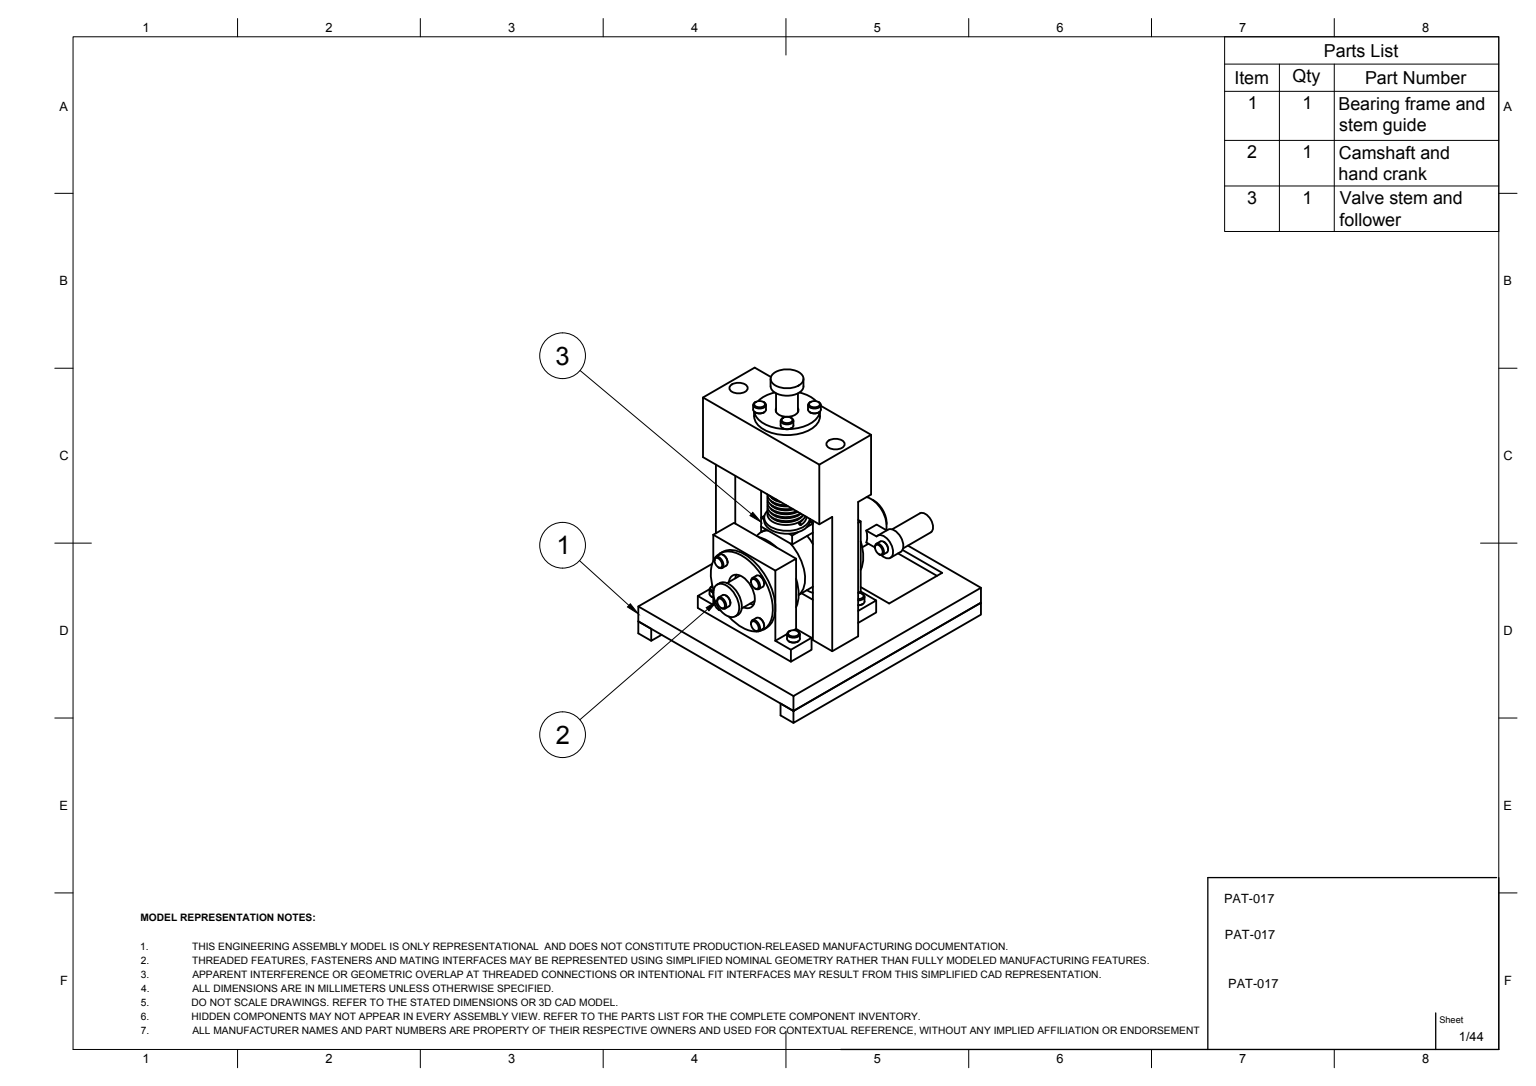
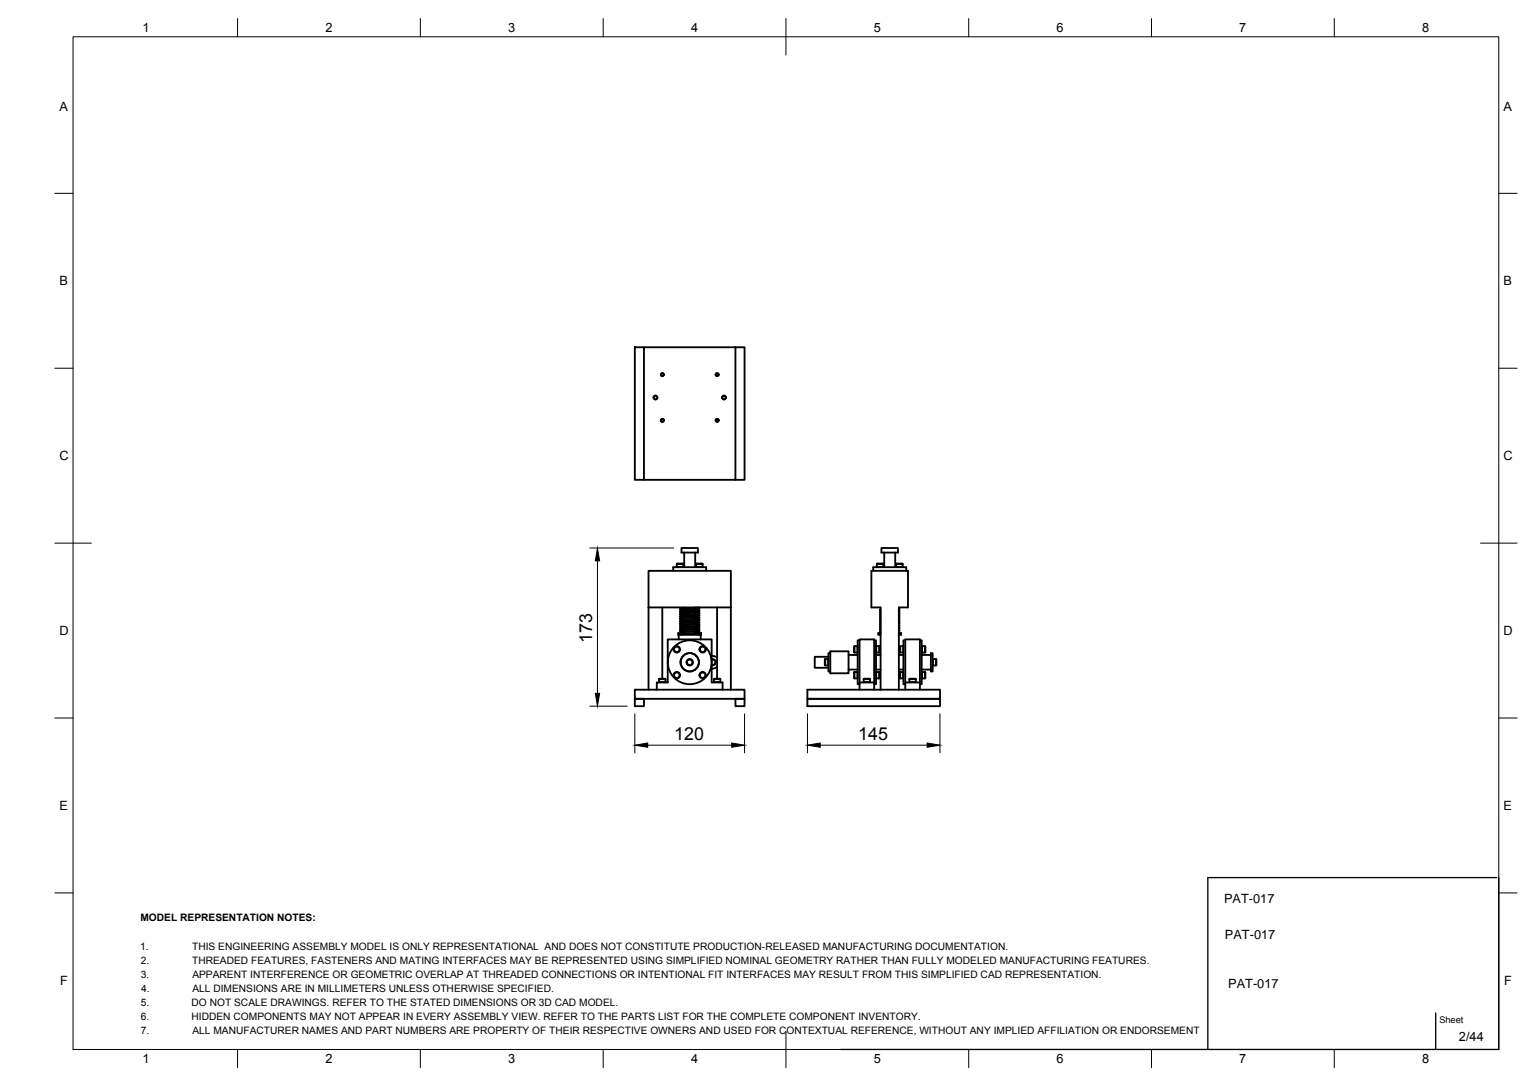
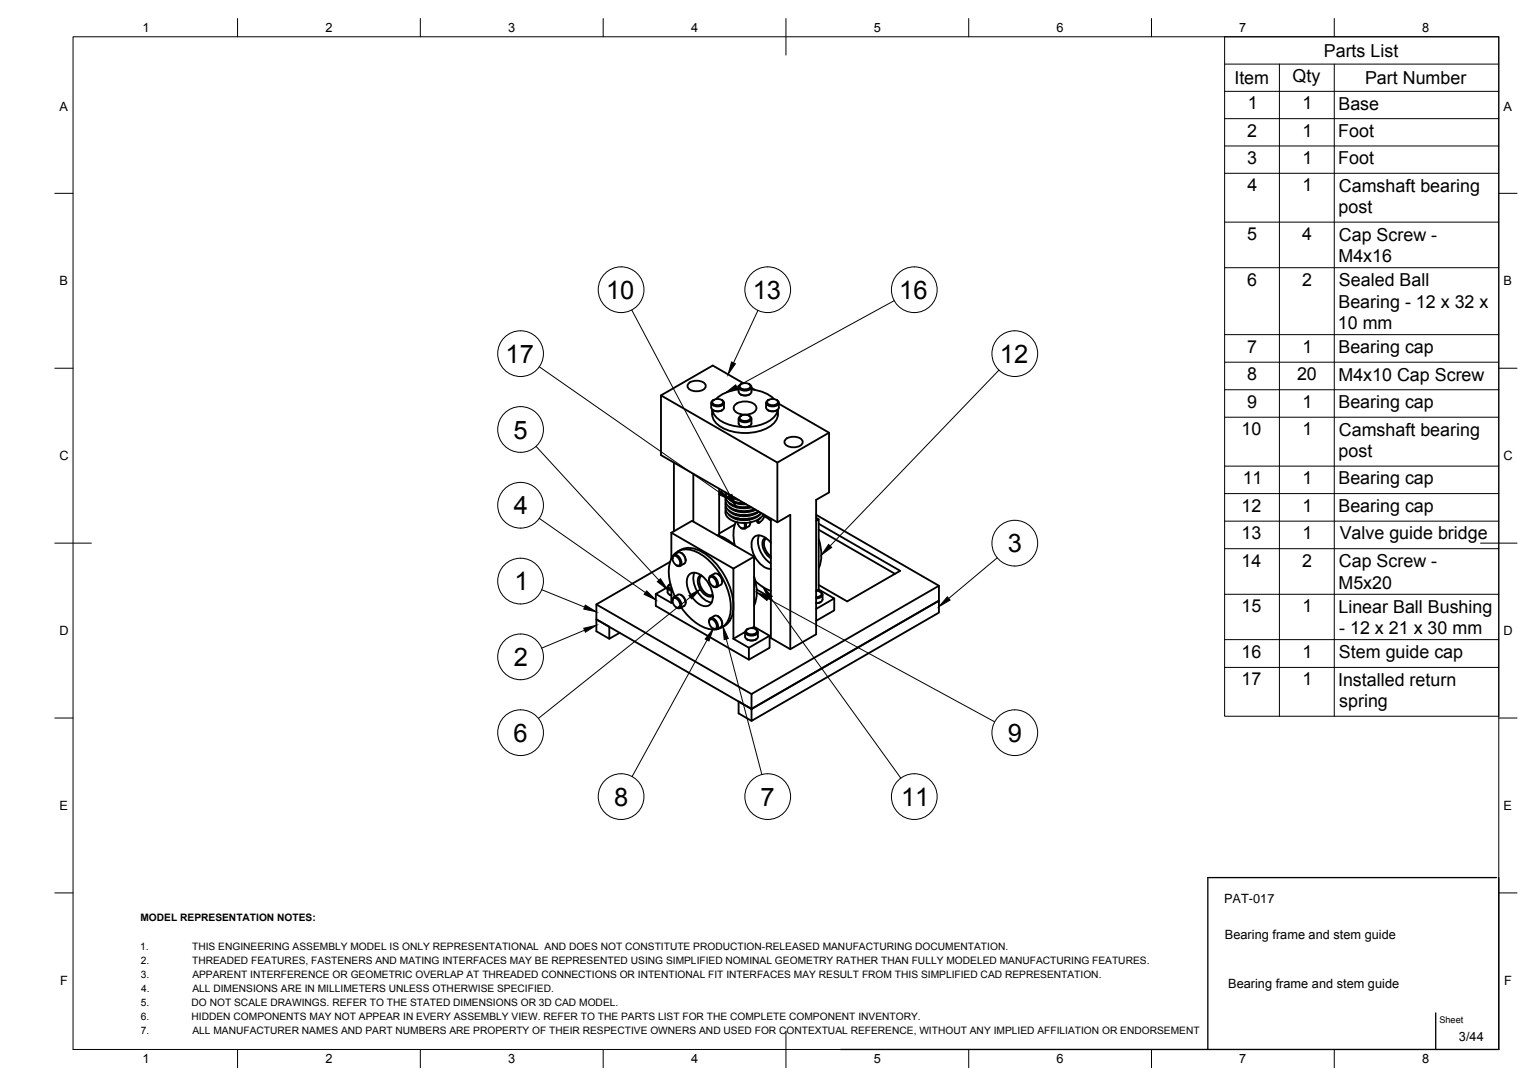
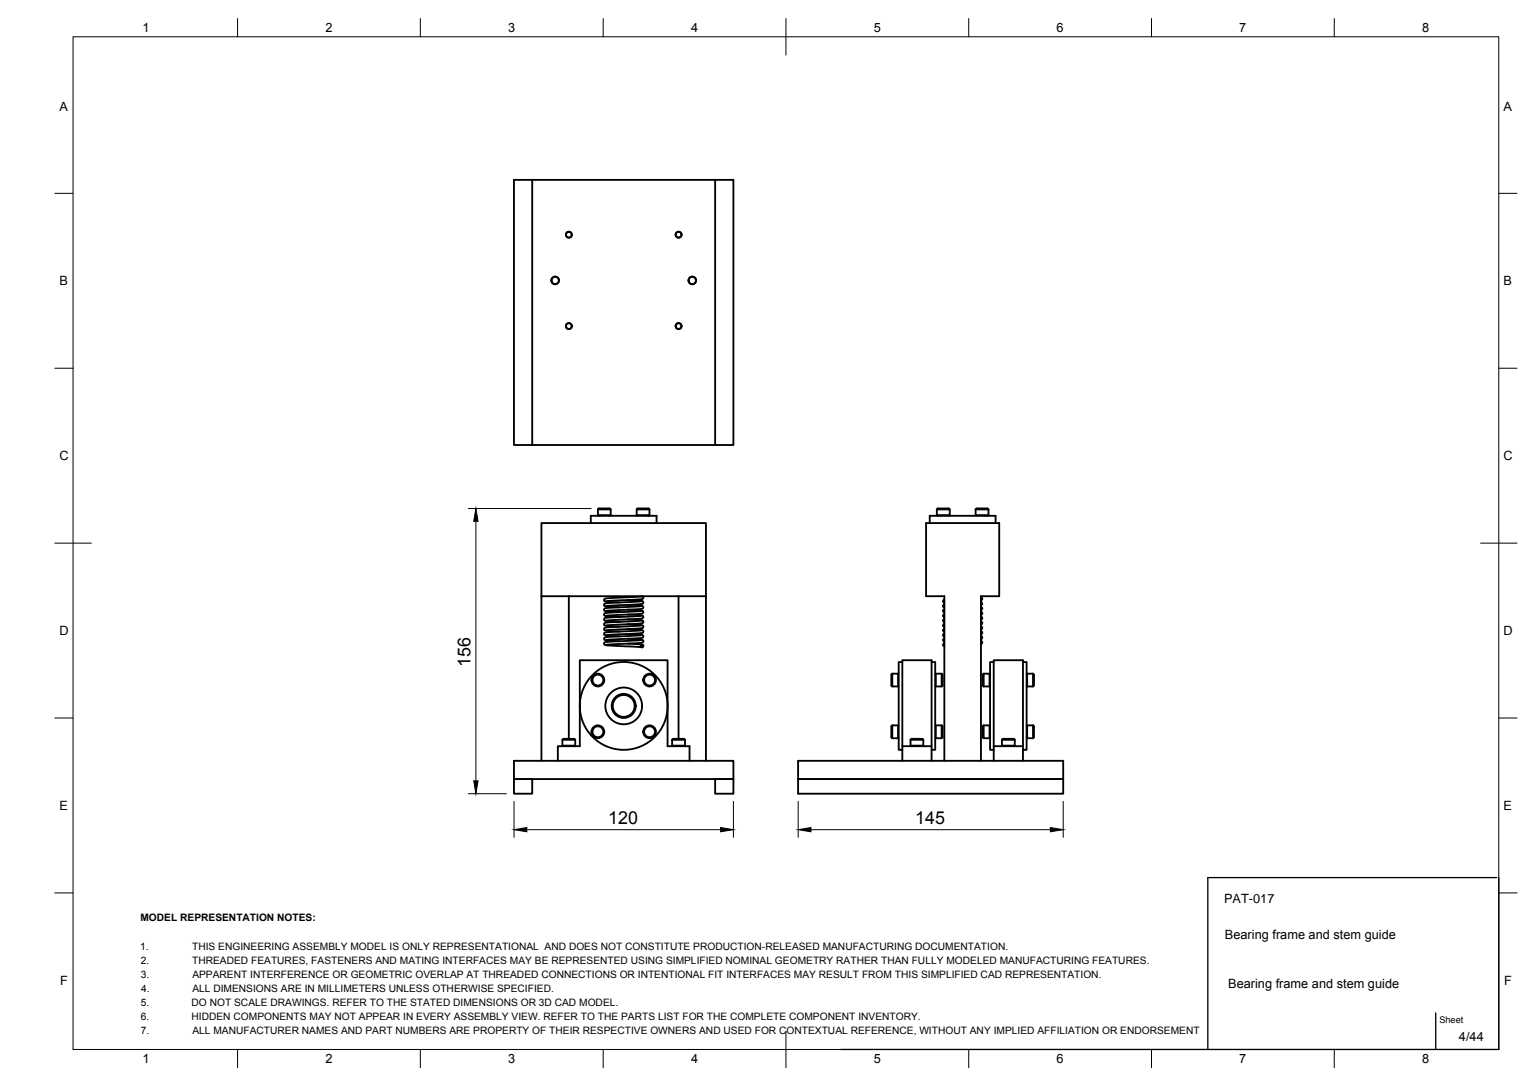
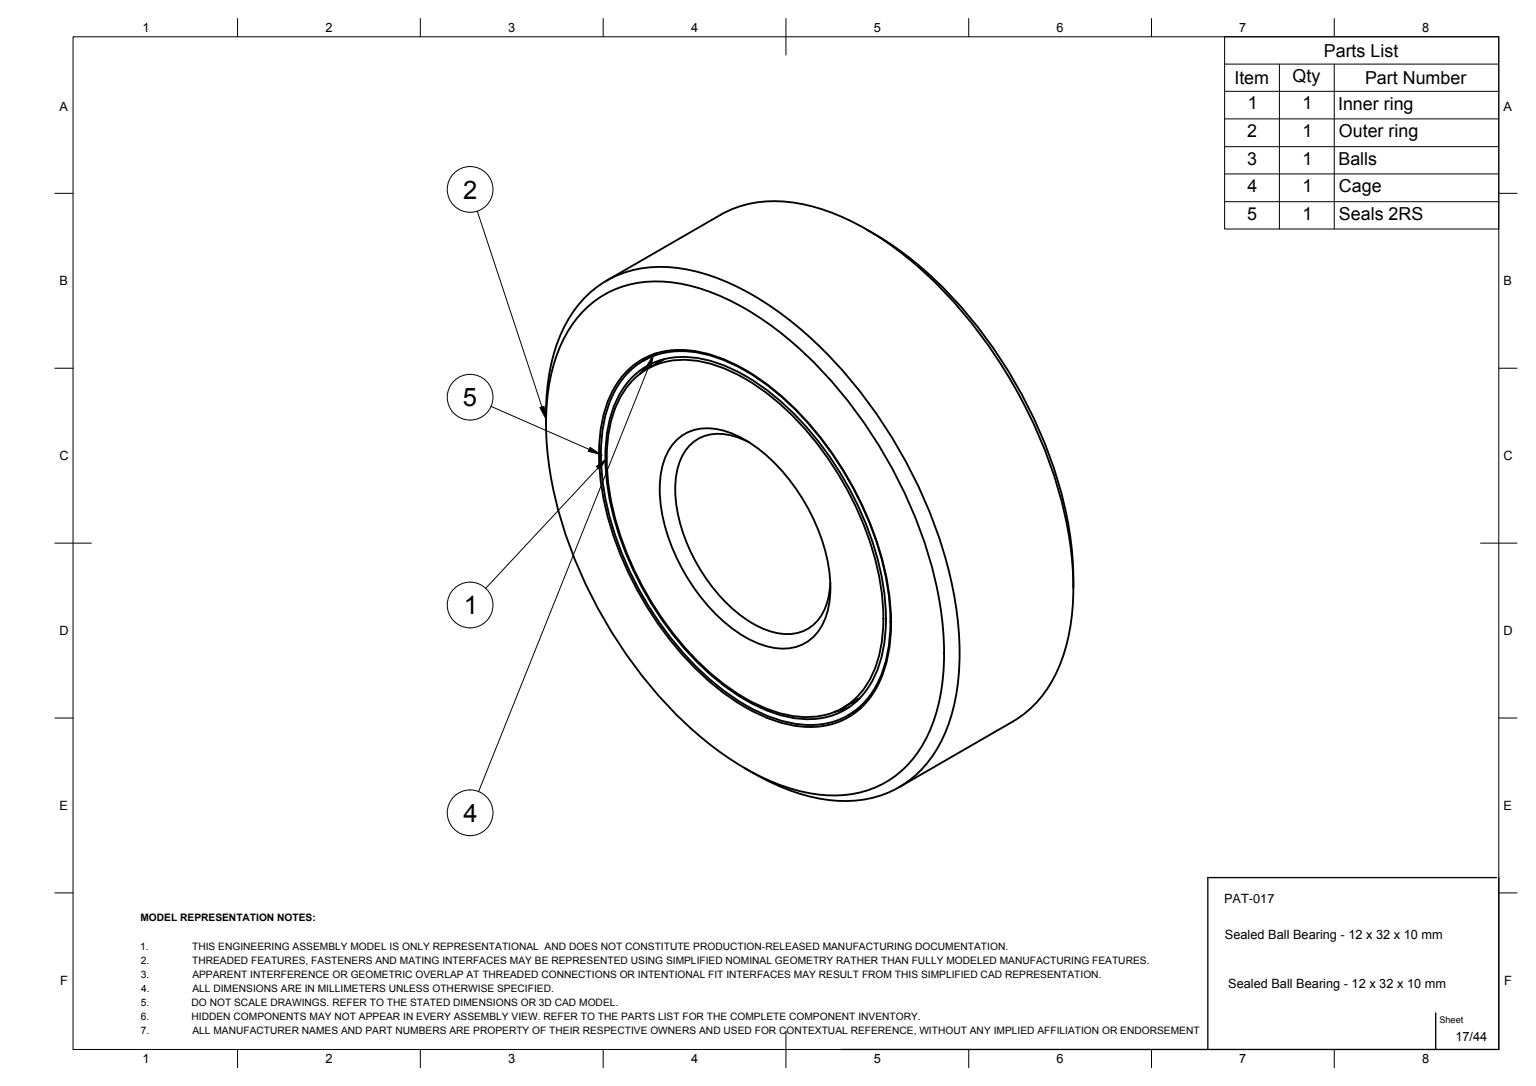
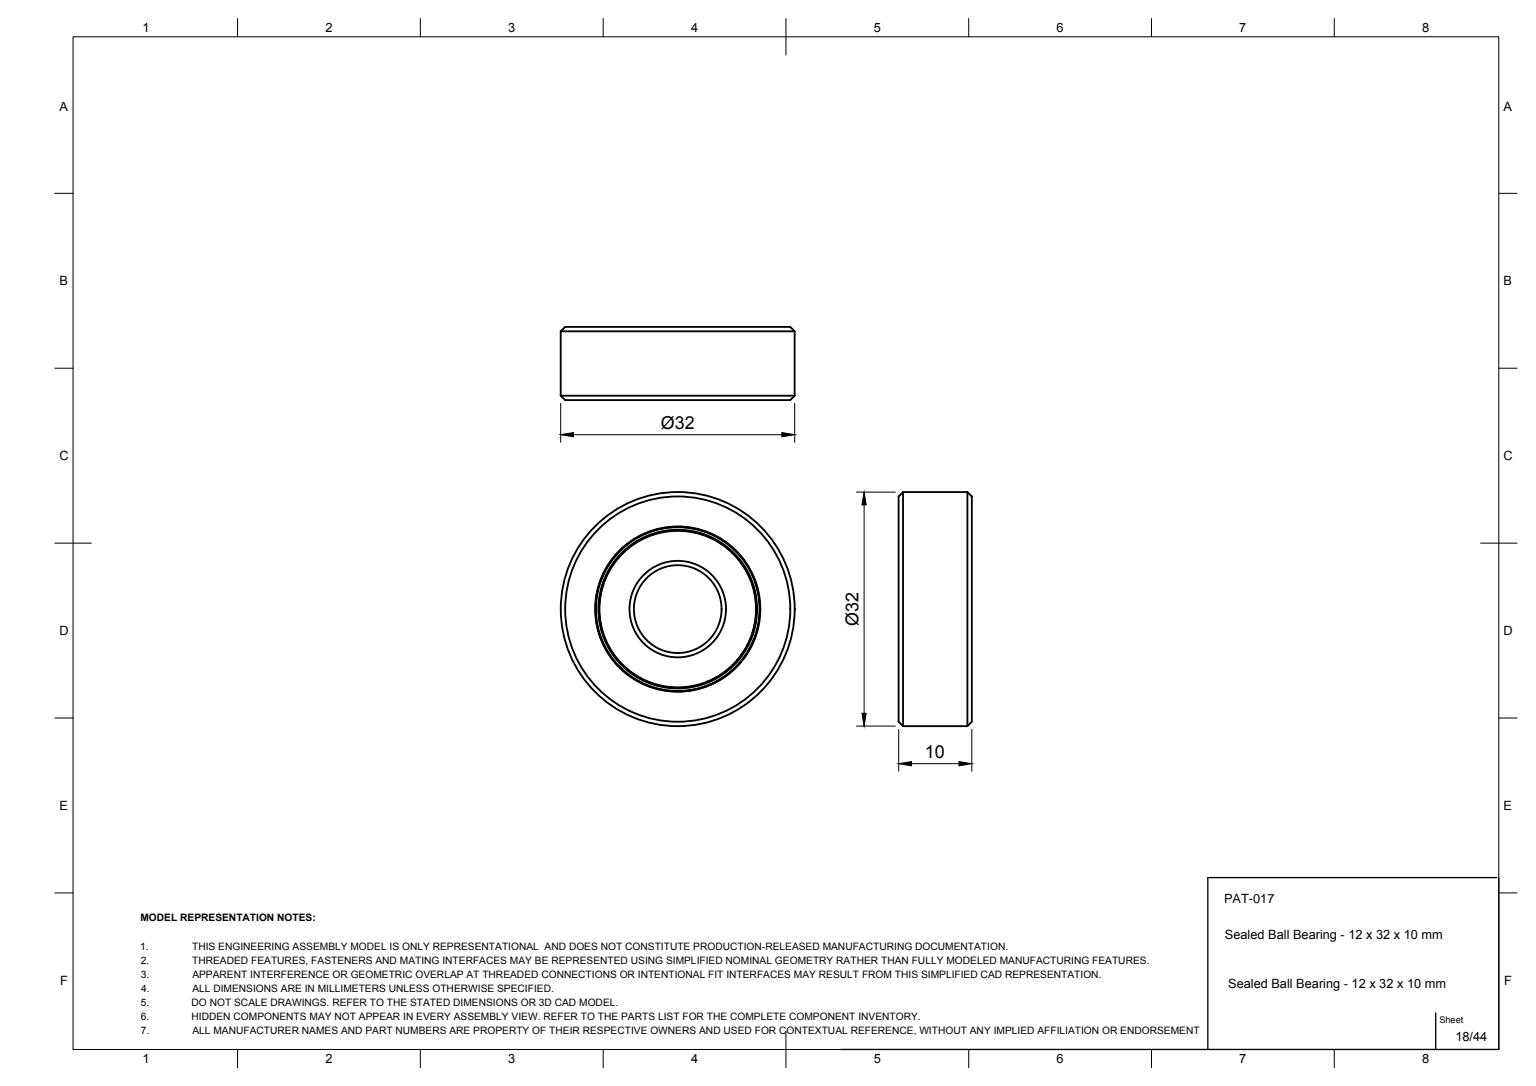
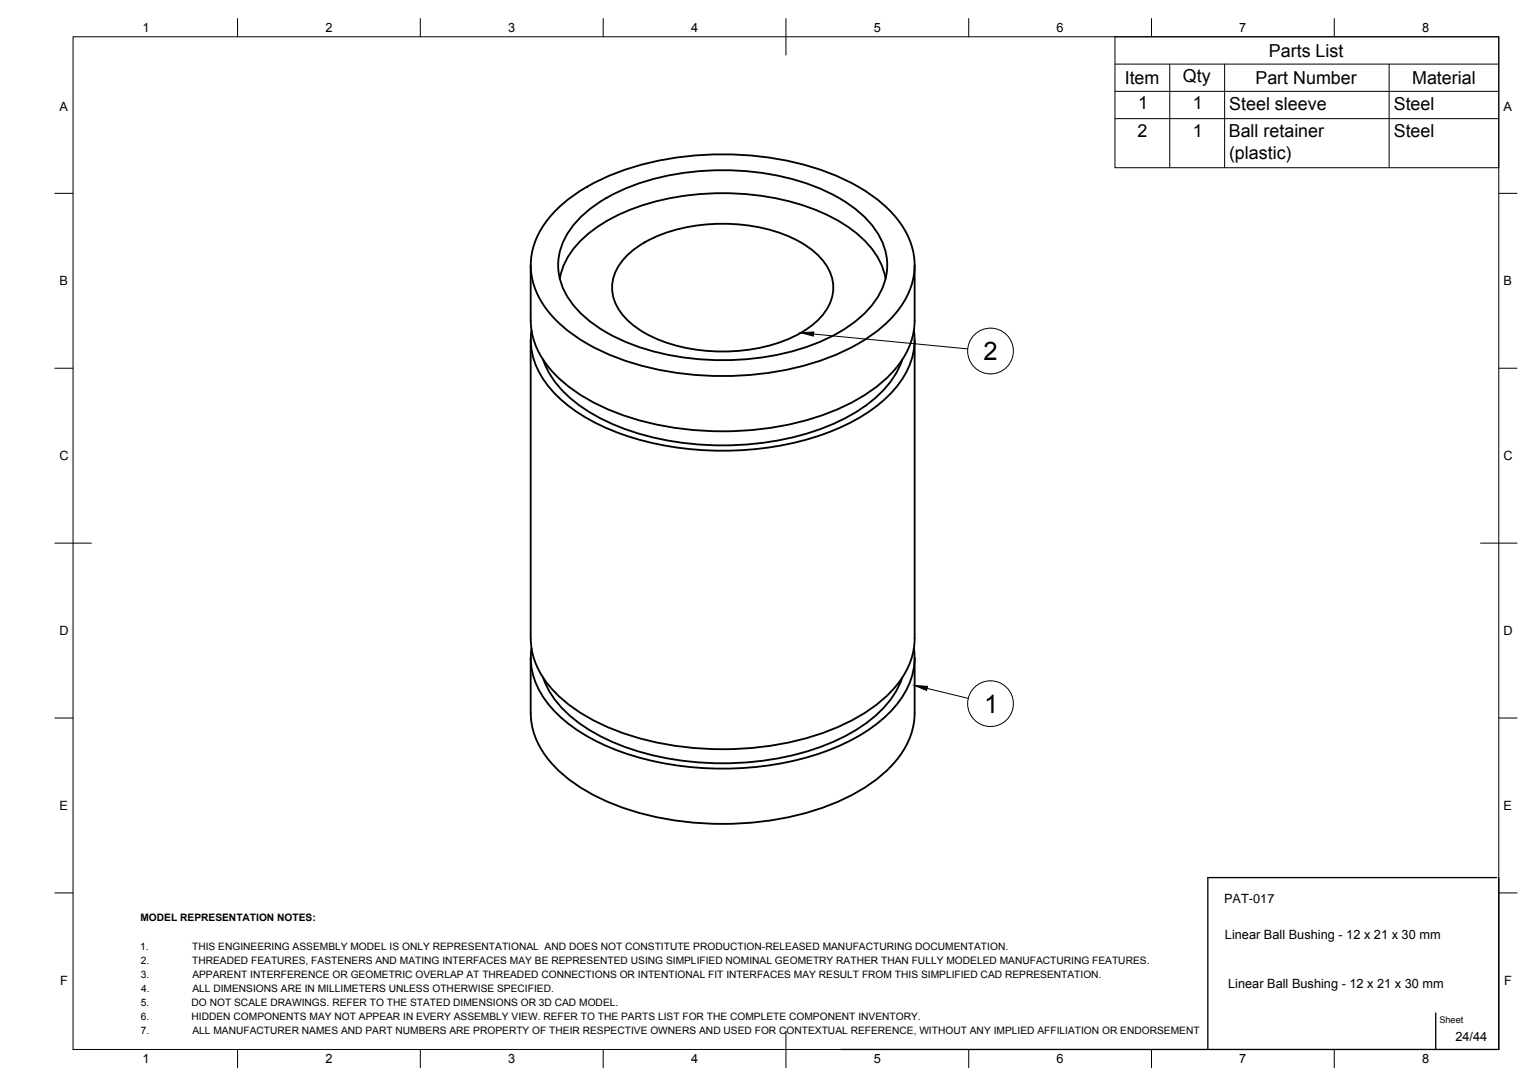
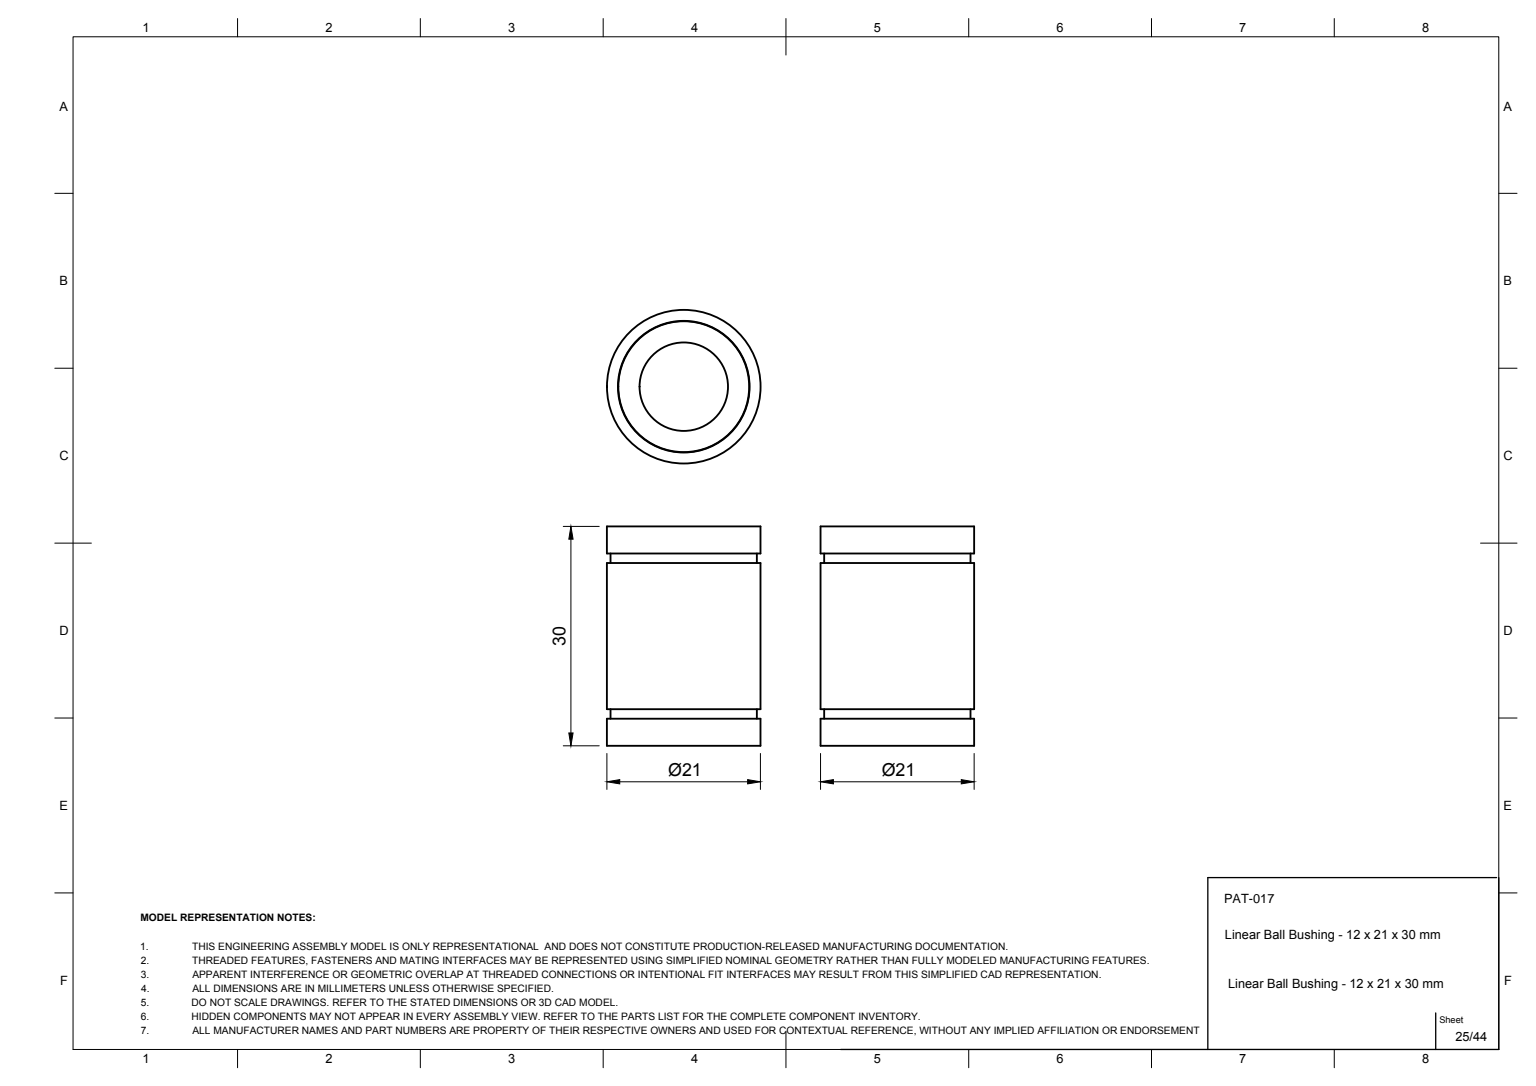
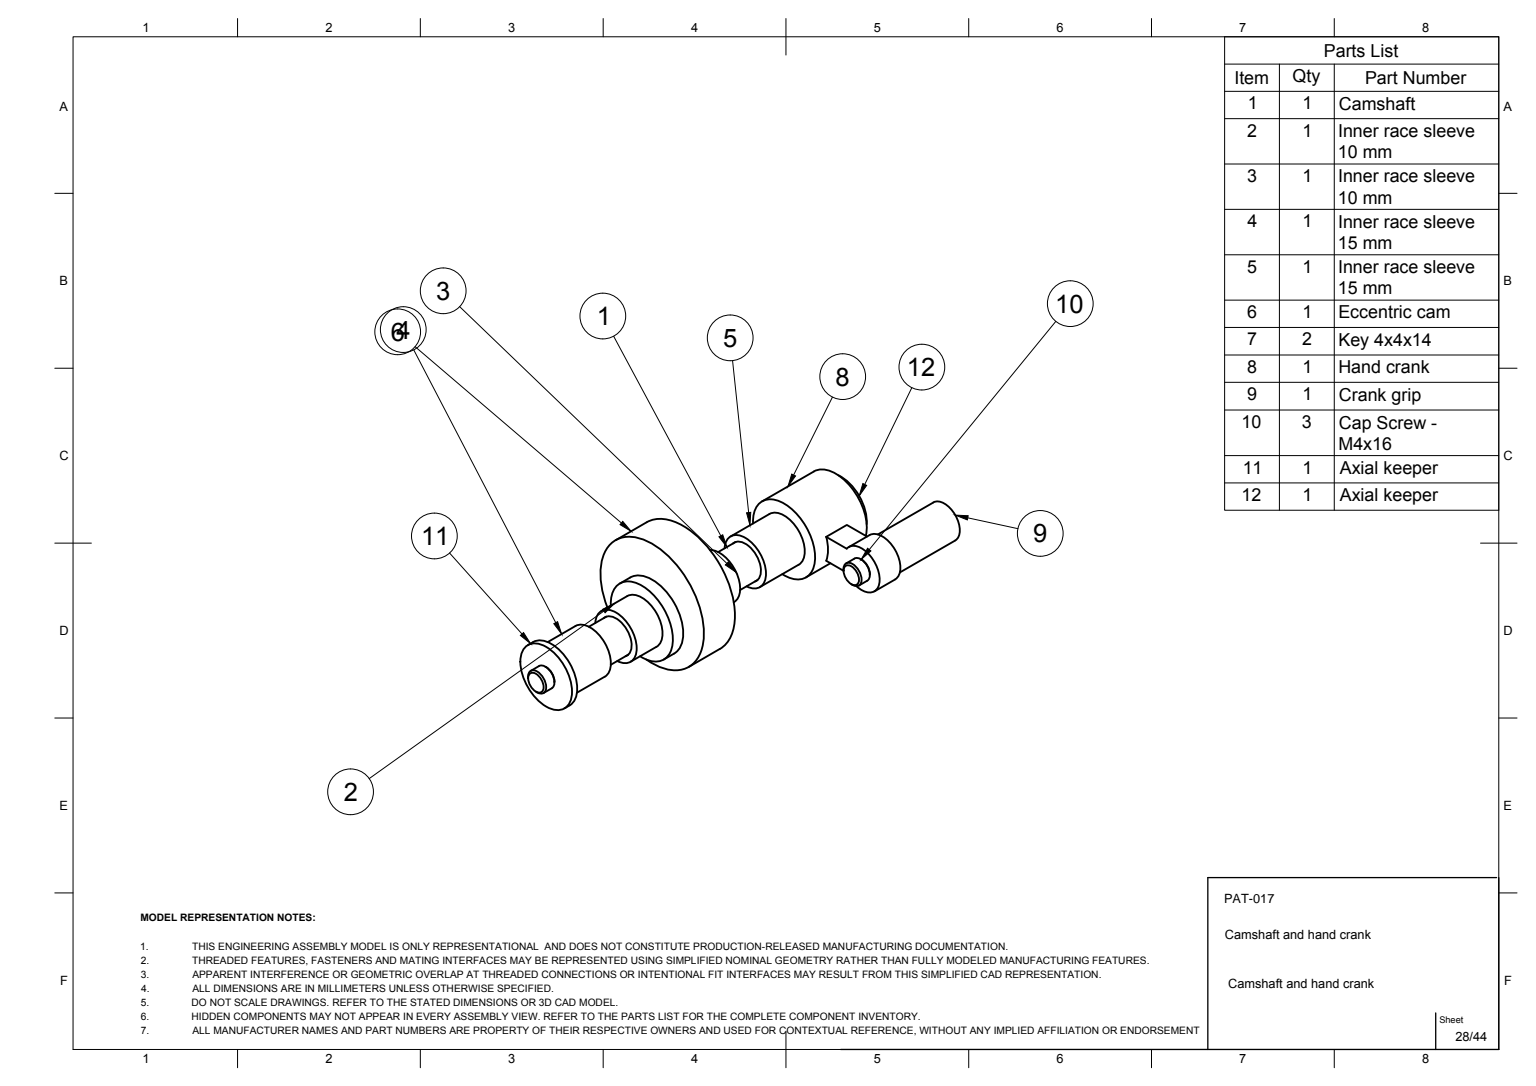
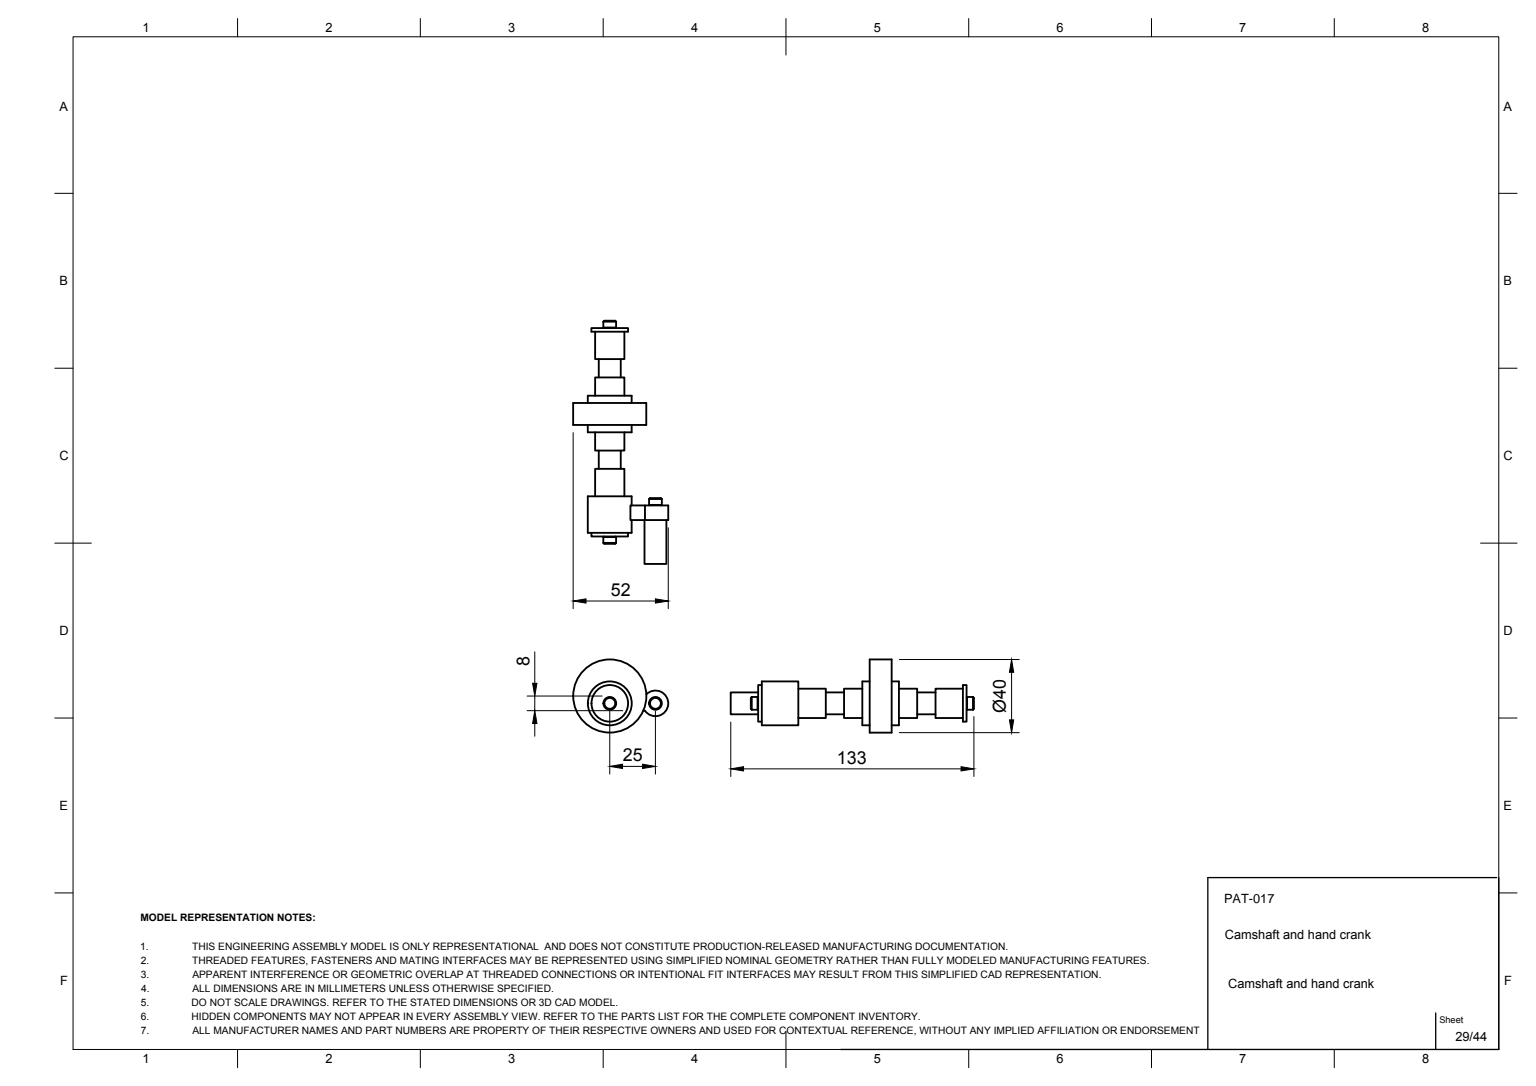
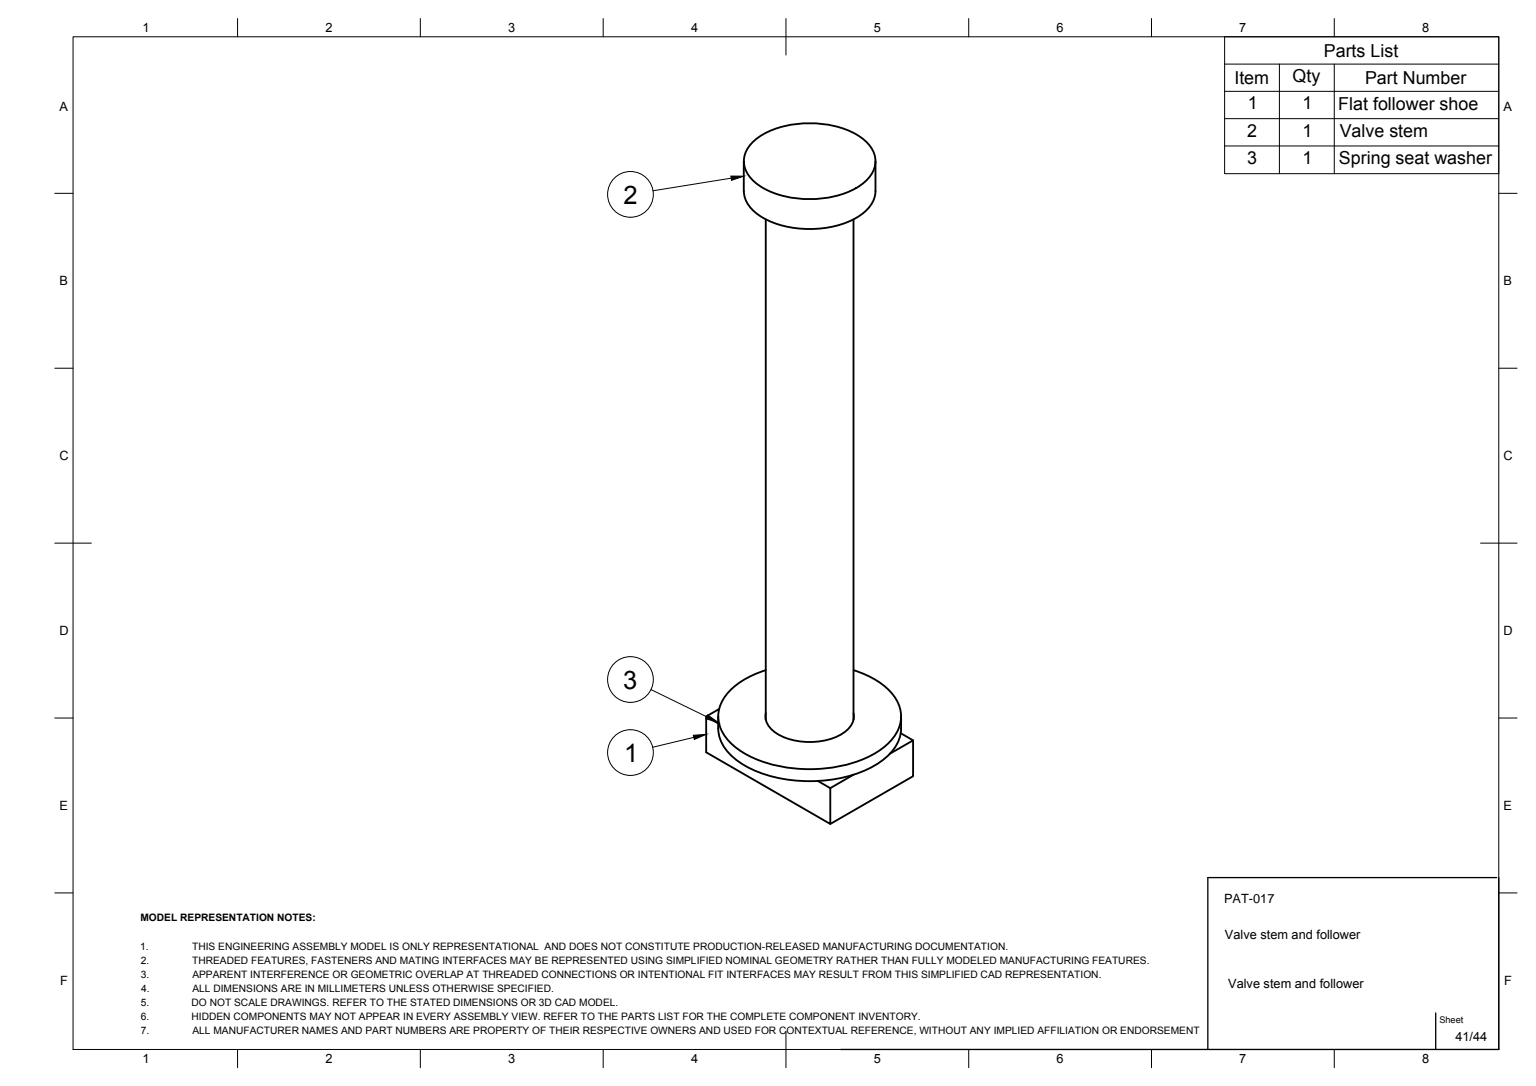
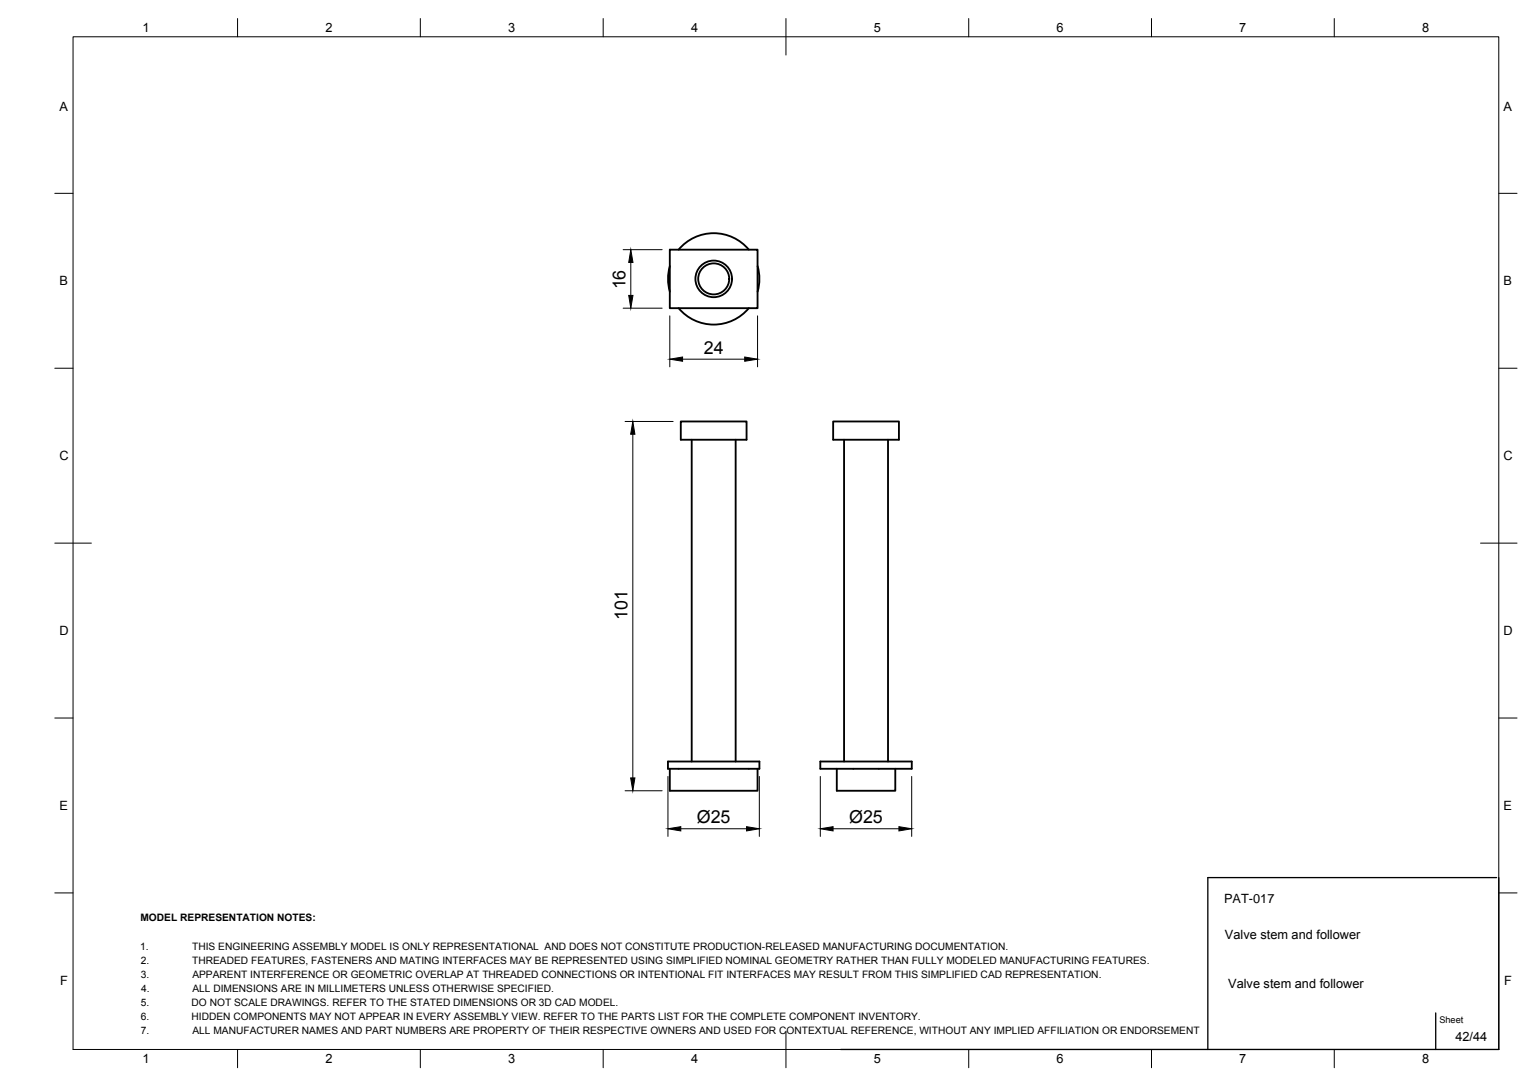
ISO-10303-21;
HEADER;
/* Generated by software containing ST-Developer
 * from STEP Tools, Inc. (www.steptools.com) 
 */

FILE_DESCRIPTION(
/* description */ ('Cam-and-follower valve demonstrator'),
/* implementation_level */ '2;1');

FILE_NAME(
/* name */ 'PAT-017',
/* time_stamp */ '2026-10-28T03:25:17-07:00',
/* author */ (''),
/* organization */ (''),
/* preprocessor_version */ 'ST-DEVELOPER v20.2',
/* originating_system */ 'Autodesk Translation Framework v15.17.0.0',
/* authorisation */ '');

FILE_SCHEMA (('AUTOMOTIVE_DESIGN { 1 0 10303 214 3 1 1 }'));
ENDSEC;

DATA;
#10=MECHANICAL_DESIGN_GEOMETRIC_PRESENTATION_REPRESENTATION('',(#412,#413,
#414,#415,#416,#417,#418,#419,#420,#421,#422,#423,#424,#425,#426,#427,#428,
#429,#430,#431,#432,#433,#434,#435,#436,#437,#438,#439,#440,#441,#442,#443,
#444,#445,#446,#447,#448,#449,#450,#451,#452,#453,#454),#12896);
#11=ORIENTED_CLOSED_SHELL('',*,#6204,.F.);
#12=ORIENTED_CLOSED_SHELL('',*,#6207,.F.);
#13=ORIENTED_CLOSED_SHELL('',*,#6221,.F.);
#14=BREP_WITH_VOIDS('Body1',#6203,(#11));
#15=BREP_WITH_VOIDS('Body1',#6208,(#12));
#16=BREP_WITH_VOIDS('Body1',#6220,(#13));
#17=ITEM_DEFINED_TRANSFORMATION($,$,#6915,#7037);
#18=ITEM_DEFINED_TRANSFORMATION($,$,#6935,#7038);
#19=ITEM_DEFINED_TRANSFORMATION($,$,#6955,#7039);
#20=ITEM_DEFINED_TRANSFORMATION($,$,#6970,#7040);
#21=ITEM_DEFINED_TRANSFORMATION($,$,#7020,#7041);
#22=ITEM_DEFINED_TRANSFORMATION($,$,#7069,#7118);
#23=ITEM_DEFINED_TRANSFORMATION($,$,#7101,#7119);
#24=ITEM_DEFINED_TRANSFORMATION($,$,#6624,#7318);
#25=ITEM_DEFINED_TRANSFORMATION($,$,#6654,#7319);
#26=ITEM_DEFINED_TRANSFORMATION($,$,#6661,#7320);
#27=ITEM_DEFINED_TRANSFORMATION($,$,#6668,#7321);
#28=ITEM_DEFINED_TRANSFORMATION($,$,#6700,#7322);
#29=ITEM_DEFINED_TRANSFORMATION($,$,#6725,#7323);
#30=ITEM_DEFINED_TRANSFORMATION($,$,#6750,#7324);
#31=ITEM_DEFINED_TRANSFORMATION($,$,#6782,#7325);
#32=ITEM_DEFINED_TRANSFORMATION($,$,#6807,#7326);
#33=ITEM_DEFINED_TRANSFORMATION($,$,#6832,#7327);
#34=ITEM_DEFINED_TRANSFORMATION($,$,#6884,#7328);
#35=ITEM_DEFINED_TRANSFORMATION($,$,#6909,#7329);
#36=ITEM_DEFINED_TRANSFORMATION($,$,#7292,#7330);
#37=ITEM_DEFINED_TRANSFORMATION($,$,#7292,#7331);
#38=ITEM_DEFINED_TRANSFORMATION($,$,#6914,#7332);
#39=ITEM_DEFINED_TRANSFORMATION($,$,#7120,#7333);
#40=ITEM_DEFINED_TRANSFORMATION($,$,#7120,#7334);
#41=ITEM_DEFINED_TRANSFORMATION($,$,#7120,#7335);
#42=ITEM_DEFINED_TRANSFORMATION($,$,#7120,#7336);
#43=ITEM_DEFINED_TRANSFORMATION($,$,#7120,#7337);
#44=ITEM_DEFINED_TRANSFORMATION($,$,#7120,#7338);
#45=ITEM_DEFINED_TRANSFORMATION($,$,#7120,#7339);
#46=ITEM_DEFINED_TRANSFORMATION($,$,#7120,#7340);
#47=ITEM_DEFINED_TRANSFORMATION($,$,#7292,#7341);
#48=ITEM_DEFINED_TRANSFORMATION($,$,#7292,#7342);
#49=ITEM_DEFINED_TRANSFORMATION($,$,#6914,#7343);
#50=ITEM_DEFINED_TRANSFORMATION($,$,#7120,#7344);
#51=ITEM_DEFINED_TRANSFORMATION($,$,#7120,#7345);
#52=ITEM_DEFINED_TRANSFORMATION($,$,#7120,#7346);
#53=ITEM_DEFINED_TRANSFORMATION($,$,#7120,#7347);
#54=ITEM_DEFINED_TRANSFORMATION($,$,#7120,#7348);
#55=ITEM_DEFINED_TRANSFORMATION($,$,#7120,#7349);
#56=ITEM_DEFINED_TRANSFORMATION($,$,#7120,#7350);
#57=ITEM_DEFINED_TRANSFORMATION($,$,#7120,#7351);
#58=ITEM_DEFINED_TRANSFORMATION($,$,#7042,#7352);
#59=ITEM_DEFINED_TRANSFORMATION($,$,#7042,#7353);
#60=ITEM_DEFINED_TRANSFORMATION($,$,#7068,#7354);
#61=ITEM_DEFINED_TRANSFORMATION($,$,#7120,#7355);
#62=ITEM_DEFINED_TRANSFORMATION($,$,#7120,#7356);
#63=ITEM_DEFINED_TRANSFORMATION($,$,#7120,#7357);
#64=ITEM_DEFINED_TRANSFORMATION($,$,#7120,#7358);
#65=ITEM_DEFINED_TRANSFORMATION($,$,#7145,#7359);
#66=ITEM_DEFINED_TRANSFORMATION($,$,#7173,#7360);
#67=ITEM_DEFINED_TRANSFORMATION($,$,#7182,#7361);
#68=ITEM_DEFINED_TRANSFORMATION($,$,#7191,#7362);
#69=ITEM_DEFINED_TRANSFORMATION($,$,#7200,#7363);
#70=ITEM_DEFINED_TRANSFORMATION($,$,#7209,#7364);
#71=ITEM_DEFINED_TRANSFORMATION($,$,#7229,#7365);
#72=ITEM_DEFINED_TRANSFORMATION($,$,#7253,#7366);
#73=ITEM_DEFINED_TRANSFORMATION($,$,#7263,#7367);
#74=ITEM_DEFINED_TRANSFORMATION($,$,#7272,#7368);
#75=ITEM_DEFINED_TRANSFORMATION($,$,#7281,#7369);
#76=ITEM_DEFINED_TRANSFORMATION($,$,#7281,#7370);
#77=ITEM_DEFINED_TRANSFORMATION($,$,#7292,#7371);
#78=ITEM_DEFINED_TRANSFORMATION($,$,#7292,#7372);
#79=ITEM_DEFINED_TRANSFORMATION($,$,#7292,#7373);
#80=ITEM_DEFINED_TRANSFORMATION($,$,#7375,#7408);
#81=ITEM_DEFINED_TRANSFORMATION($,$,#7385,#7409);
#82=ITEM_DEFINED_TRANSFORMATION($,$,#7399,#7410);
#83=ITEM_DEFINED_TRANSFORMATION($,$,#6623,#7411);
#84=ITEM_DEFINED_TRANSFORMATION($,$,#7144,#7412);
#85=ITEM_DEFINED_TRANSFORMATION($,$,#7374,#7413);
#86=(
REPRESENTATION_RELATIONSHIP($,$,#13069,#13068)
REPRESENTATION_RELATIONSHIP_WITH_TRANSFORMATION(#17)
SHAPE_REPRESENTATION_RELATIONSHIP()
);
#87=(
REPRESENTATION_RELATIONSHIP($,$,#13070,#13068)
REPRESENTATION_RELATIONSHIP_WITH_TRANSFORMATION(#18)
SHAPE_REPRESENTATION_RELATIONSHIP()
);
#88=(
REPRESENTATION_RELATIONSHIP($,$,#13071,#13068)
REPRESENTATION_RELATIONSHIP_WITH_TRANSFORMATION(#19)
SHAPE_REPRESENTATION_RELATIONSHIP()
);
#89=(
REPRESENTATION_RELATIONSHIP($,$,#13072,#13068)
REPRESENTATION_RELATIONSHIP_WITH_TRANSFORMATION(#20)
SHAPE_REPRESENTATION_RELATIONSHIP()
);
#90=(
REPRESENTATION_RELATIONSHIP($,$,#13073,#13068)
REPRESENTATION_RELATIONSHIP_WITH_TRANSFORMATION(#21)
SHAPE_REPRESENTATION_RELATIONSHIP()
);
#91=(
REPRESENTATION_RELATIONSHIP($,$,#13076,#13075)
REPRESENTATION_RELATIONSHIP_WITH_TRANSFORMATION(#22)
SHAPE_REPRESENTATION_RELATIONSHIP()
);
#92=(
REPRESENTATION_RELATIONSHIP($,$,#13077,#13075)
REPRESENTATION_RELATIONSHIP_WITH_TRANSFORMATION(#23)
SHAPE_REPRESENTATION_RELATIONSHIP()
);
#93=(
REPRESENTATION_RELATIONSHIP($,$,#13056,#13055)
REPRESENTATION_RELATIONSHIP_WITH_TRANSFORMATION(#24)
SHAPE_REPRESENTATION_RELATIONSHIP()
);
#94=(
REPRESENTATION_RELATIONSHIP($,$,#13057,#13055)
REPRESENTATION_RELATIONSHIP_WITH_TRANSFORMATION(#25)
SHAPE_REPRESENTATION_RELATIONSHIP()
);
#95=(
REPRESENTATION_RELATIONSHIP($,$,#13058,#13055)
REPRESENTATION_RELATIONSHIP_WITH_TRANSFORMATION(#26)
SHAPE_REPRESENTATION_RELATIONSHIP()
);
#96=(
REPRESENTATION_RELATIONSHIP($,$,#13059,#13055)
REPRESENTATION_RELATIONSHIP_WITH_TRANSFORMATION(#27)
SHAPE_REPRESENTATION_RELATIONSHIP()
);
#97=(
REPRESENTATION_RELATIONSHIP($,$,#13060,#13055)
REPRESENTATION_RELATIONSHIP_WITH_TRANSFORMATION(#28)
SHAPE_REPRESENTATION_RELATIONSHIP()
);
#98=(
REPRESENTATION_RELATIONSHIP($,$,#13061,#13055)
REPRESENTATION_RELATIONSHIP_WITH_TRANSFORMATION(#29)
SHAPE_REPRESENTATION_RELATIONSHIP()
);
#99=(
REPRESENTATION_RELATIONSHIP($,$,#13062,#13055)
REPRESENTATION_RELATIONSHIP_WITH_TRANSFORMATION(#30)
SHAPE_REPRESENTATION_RELATIONSHIP()
);
#100=(
REPRESENTATION_RELATIONSHIP($,$,#13063,#13055)
REPRESENTATION_RELATIONSHIP_WITH_TRANSFORMATION(#31)
SHAPE_REPRESENTATION_RELATIONSHIP()
);
#101=(
REPRESENTATION_RELATIONSHIP($,$,#13064,#13055)
REPRESENTATION_RELATIONSHIP_WITH_TRANSFORMATION(#32)
SHAPE_REPRESENTATION_RELATIONSHIP()
);
#102=(
REPRESENTATION_RELATIONSHIP($,$,#13065,#13055)
REPRESENTATION_RELATIONSHIP_WITH_TRANSFORMATION(#33)
SHAPE_REPRESENTATION_RELATIONSHIP()
);
#103=(
REPRESENTATION_RELATIONSHIP($,$,#13066,#13055)
REPRESENTATION_RELATIONSHIP_WITH_TRANSFORMATION(#34)
SHAPE_REPRESENTATION_RELATIONSHIP()
);
#104=(
REPRESENTATION_RELATIONSHIP($,$,#13067,#13055)
REPRESENTATION_RELATIONSHIP_WITH_TRANSFORMATION(#35)
SHAPE_REPRESENTATION_RELATIONSHIP()
);
#105=(
REPRESENTATION_RELATIONSHIP($,$,#13091,#13055)
REPRESENTATION_RELATIONSHIP_WITH_TRANSFORMATION(#36)
SHAPE_REPRESENTATION_RELATIONSHIP()
);
#106=(
REPRESENTATION_RELATIONSHIP($,$,#13091,#13055)
REPRESENTATION_RELATIONSHIP_WITH_TRANSFORMATION(#37)
SHAPE_REPRESENTATION_RELATIONSHIP()
);
#107=(
REPRESENTATION_RELATIONSHIP($,$,#13068,#13055)
REPRESENTATION_RELATIONSHIP_WITH_TRANSFORMATION(#38)
SHAPE_REPRESENTATION_RELATIONSHIP()
);
#108=(
REPRESENTATION_RELATIONSHIP($,$,#13078,#13055)
REPRESENTATION_RELATIONSHIP_WITH_TRANSFORMATION(#39)
SHAPE_REPRESENTATION_RELATIONSHIP()
);
#109=(
REPRESENTATION_RELATIONSHIP($,$,#13078,#13055)
REPRESENTATION_RELATIONSHIP_WITH_TRANSFORMATION(#40)
SHAPE_REPRESENTATION_RELATIONSHIP()
);
#110=(
REPRESENTATION_RELATIONSHIP($,$,#13078,#13055)
REPRESENTATION_RELATIONSHIP_WITH_TRANSFORMATION(#41)
SHAPE_REPRESENTATION_RELATIONSHIP()
);
#111=(
REPRESENTATION_RELATIONSHIP($,$,#13078,#13055)
REPRESENTATION_RELATIONSHIP_WITH_TRANSFORMATION(#42)
SHAPE_REPRESENTATION_RELATIONSHIP()
);
#112=(
REPRESENTATION_RELATIONSHIP($,$,#13078,#13055)
REPRESENTATION_RELATIONSHIP_WITH_TRANSFORMATION(#43)
SHAPE_REPRESENTATION_RELATIONSHIP()
);
#113=(
REPRESENTATION_RELATIONSHIP($,$,#13078,#13055)
REPRESENTATION_RELATIONSHIP_WITH_TRANSFORMATION(#44)
SHAPE_REPRESENTATION_RELATIONSHIP()
);
#114=(
REPRESENTATION_RELATIONSHIP($,$,#13078,#13055)
REPRESENTATION_RELATIONSHIP_WITH_TRANSFORMATION(#45)
SHAPE_REPRESENTATION_RELATIONSHIP()
);
#115=(
REPRESENTATION_RELATIONSHIP($,$,#13078,#13055)
REPRESENTATION_RELATIONSHIP_WITH_TRANSFORMATION(#46)
SHAPE_REPRESENTATION_RELATIONSHIP()
);
#116=(
REPRESENTATION_RELATIONSHIP($,$,#13091,#13055)
REPRESENTATION_RELATIONSHIP_WITH_TRANSFORMATION(#47)
SHAPE_REPRESENTATION_RELATIONSHIP()
);
#117=(
REPRESENTATION_RELATIONSHIP($,$,#13091,#13055)
REPRESENTATION_RELATIONSHIP_WITH_TRANSFORMATION(#48)
SHAPE_REPRESENTATION_RELATIONSHIP()
);
#118=(
REPRESENTATION_RELATIONSHIP($,$,#13068,#13055)
REPRESENTATION_RELATIONSHIP_WITH_TRANSFORMATION(#49)
SHAPE_REPRESENTATION_RELATIONSHIP()
);
#119=(
REPRESENTATION_RELATIONSHIP($,$,#13078,#13055)
REPRESENTATION_RELATIONSHIP_WITH_TRANSFORMATION(#50)
SHAPE_REPRESENTATION_RELATIONSHIP()
);
#120=(
REPRESENTATION_RELATIONSHIP($,$,#13078,#13055)
REPRESENTATION_RELATIONSHIP_WITH_TRANSFORMATION(#51)
SHAPE_REPRESENTATION_RELATIONSHIP()
);
#121=(
REPRESENTATION_RELATIONSHIP($,$,#13078,#13055)
REPRESENTATION_RELATIONSHIP_WITH_TRANSFORMATION(#52)
SHAPE_REPRESENTATION_RELATIONSHIP()
);
#122=(
REPRESENTATION_RELATIONSHIP($,$,#13078,#13055)
REPRESENTATION_RELATIONSHIP_WITH_TRANSFORMATION(#53)
SHAPE_REPRESENTATION_RELATIONSHIP()
);
#123=(
REPRESENTATION_RELATIONSHIP($,$,#13078,#13055)
REPRESENTATION_RELATIONSHIP_WITH_TRANSFORMATION(#54)
SHAPE_REPRESENTATION_RELATIONSHIP()
);
#124=(
REPRESENTATION_RELATIONSHIP($,$,#13078,#13055)
REPRESENTATION_RELATIONSHIP_WITH_TRANSFORMATION(#55)
SHAPE_REPRESENTATION_RELATIONSHIP()
);
#125=(
REPRESENTATION_RELATIONSHIP($,$,#13078,#13055)
REPRESENTATION_RELATIONSHIP_WITH_TRANSFORMATION(#56)
SHAPE_REPRESENTATION_RELATIONSHIP()
);
#126=(
REPRESENTATION_RELATIONSHIP($,$,#13078,#13055)
REPRESENTATION_RELATIONSHIP_WITH_TRANSFORMATION(#57)
SHAPE_REPRESENTATION_RELATIONSHIP()
);
#127=(
REPRESENTATION_RELATIONSHIP($,$,#13074,#13055)
REPRESENTATION_RELATIONSHIP_WITH_TRANSFORMATION(#58)
SHAPE_REPRESENTATION_RELATIONSHIP()
);
#128=(
REPRESENTATION_RELATIONSHIP($,$,#13074,#13055)
REPRESENTATION_RELATIONSHIP_WITH_TRANSFORMATION(#59)
SHAPE_REPRESENTATION_RELATIONSHIP()
);
#129=(
REPRESENTATION_RELATIONSHIP($,$,#13075,#13055)
REPRESENTATION_RELATIONSHIP_WITH_TRANSFORMATION(#60)
SHAPE_REPRESENTATION_RELATIONSHIP()
);
#130=(
REPRESENTATION_RELATIONSHIP($,$,#13078,#13055)
REPRESENTATION_RELATIONSHIP_WITH_TRANSFORMATION(#61)
SHAPE_REPRESENTATION_RELATIONSHIP()
);
#131=(
REPRESENTATION_RELATIONSHIP($,$,#13078,#13055)
REPRESENTATION_RELATIONSHIP_WITH_TRANSFORMATION(#62)
SHAPE_REPRESENTATION_RELATIONSHIP()
);
#132=(
REPRESENTATION_RELATIONSHIP($,$,#13078,#13055)
REPRESENTATION_RELATIONSHIP_WITH_TRANSFORMATION(#63)
SHAPE_REPRESENTATION_RELATIONSHIP()
);
#133=(
REPRESENTATION_RELATIONSHIP($,$,#13078,#13055)
REPRESENTATION_RELATIONSHIP_WITH_TRANSFORMATION(#64)
SHAPE_REPRESENTATION_RELATIONSHIP()
);
#134=(
REPRESENTATION_RELATIONSHIP($,$,#13080,#13079)
REPRESENTATION_RELATIONSHIP_WITH_TRANSFORMATION(#65)
SHAPE_REPRESENTATION_RELATIONSHIP()
);
#135=(
REPRESENTATION_RELATIONSHIP($,$,#13081,#13079)
REPRESENTATION_RELATIONSHIP_WITH_TRANSFORMATION(#66)
SHAPE_REPRESENTATION_RELATIONSHIP()
);
#136=(
REPRESENTATION_RELATIONSHIP($,$,#13082,#13079)
REPRESENTATION_RELATIONSHIP_WITH_TRANSFORMATION(#67)
SHAPE_REPRESENTATION_RELATIONSHIP()
);
#137=(
REPRESENTATION_RELATIONSHIP($,$,#13083,#13079)
REPRESENTATION_RELATIONSHIP_WITH_TRANSFORMATION(#68)
SHAPE_REPRESENTATION_RELATIONSHIP()
);
#138=(
REPRESENTATION_RELATIONSHIP($,$,#13084,#13079)
REPRESENTATION_RELATIONSHIP_WITH_TRANSFORMATION(#69)
SHAPE_REPRESENTATION_RELATIONSHIP()
);
#139=(
REPRESENTATION_RELATIONSHIP($,$,#13085,#13079)
REPRESENTATION_RELATIONSHIP_WITH_TRANSFORMATION(#70)
SHAPE_REPRESENTATION_RELATIONSHIP()
);
#140=(
REPRESENTATION_RELATIONSHIP($,$,#13086,#13079)
REPRESENTATION_RELATIONSHIP_WITH_TRANSFORMATION(#71)
SHAPE_REPRESENTATION_RELATIONSHIP()
);
#141=(
REPRESENTATION_RELATIONSHIP($,$,#13087,#13079)
REPRESENTATION_RELATIONSHIP_WITH_TRANSFORMATION(#72)
SHAPE_REPRESENTATION_RELATIONSHIP()
);
#142=(
REPRESENTATION_RELATIONSHIP($,$,#13088,#13079)
REPRESENTATION_RELATIONSHIP_WITH_TRANSFORMATION(#73)
SHAPE_REPRESENTATION_RELATIONSHIP()
);
#143=(
REPRESENTATION_RELATIONSHIP($,$,#13089,#13079)
REPRESENTATION_RELATIONSHIP_WITH_TRANSFORMATION(#74)
SHAPE_REPRESENTATION_RELATIONSHIP()
);
#144=(
REPRESENTATION_RELATIONSHIP($,$,#13090,#13079)
REPRESENTATION_RELATIONSHIP_WITH_TRANSFORMATION(#75)
SHAPE_REPRESENTATION_RELATIONSHIP()
);
#145=(
REPRESENTATION_RELATIONSHIP($,$,#13090,#13079)
REPRESENTATION_RELATIONSHIP_WITH_TRANSFORMATION(#76)
SHAPE_REPRESENTATION_RELATIONSHIP()
);
#146=(
REPRESENTATION_RELATIONSHIP($,$,#13091,#13079)
REPRESENTATION_RELATIONSHIP_WITH_TRANSFORMATION(#77)
SHAPE_REPRESENTATION_RELATIONSHIP()
);
#147=(
REPRESENTATION_RELATIONSHIP($,$,#13091,#13079)
REPRESENTATION_RELATIONSHIP_WITH_TRANSFORMATION(#78)
SHAPE_REPRESENTATION_RELATIONSHIP()
);
#148=(
REPRESENTATION_RELATIONSHIP($,$,#13091,#13079)
REPRESENTATION_RELATIONSHIP_WITH_TRANSFORMATION(#79)
SHAPE_REPRESENTATION_RELATIONSHIP()
);
#149=(
REPRESENTATION_RELATIONSHIP($,$,#13093,#13092)
REPRESENTATION_RELATIONSHIP_WITH_TRANSFORMATION(#80)
SHAPE_REPRESENTATION_RELATIONSHIP()
);
#150=(
REPRESENTATION_RELATIONSHIP($,$,#13094,#13092)
REPRESENTATION_RELATIONSHIP_WITH_TRANSFORMATION(#81)
SHAPE_REPRESENTATION_RELATIONSHIP()
);
#151=(
REPRESENTATION_RELATIONSHIP($,$,#13095,#13092)
REPRESENTATION_RELATIONSHIP_WITH_TRANSFORMATION(#82)
SHAPE_REPRESENTATION_RELATIONSHIP()
);
#152=(
REPRESENTATION_RELATIONSHIP($,$,#13055,#13054)
REPRESENTATION_RELATIONSHIP_WITH_TRANSFORMATION(#83)
SHAPE_REPRESENTATION_RELATIONSHIP()
);
#153=(
REPRESENTATION_RELATIONSHIP($,$,#13079,#13054)
REPRESENTATION_RELATIONSHIP_WITH_TRANSFORMATION(#84)
SHAPE_REPRESENTATION_RELATIONSHIP()
);
#154=(
REPRESENTATION_RELATIONSHIP($,$,#13092,#13054)
REPRESENTATION_RELATIONSHIP_WITH_TRANSFORMATION(#85)
SHAPE_REPRESENTATION_RELATIONSHIP()
);
#155=CONTEXT_DEPENDENT_SHAPE_REPRESENTATION(#86,#12963);
#156=CONTEXT_DEPENDENT_SHAPE_REPRESENTATION(#87,#12964);
#157=CONTEXT_DEPENDENT_SHAPE_REPRESENTATION(#88,#12965);
#158=CONTEXT_DEPENDENT_SHAPE_REPRESENTATION(#89,#12966);
#159=CONTEXT_DEPENDENT_SHAPE_REPRESENTATION(#90,#12967);
#160=CONTEXT_DEPENDENT_SHAPE_REPRESENTATION(#91,#12972);
#161=CONTEXT_DEPENDENT_SHAPE_REPRESENTATION(#92,#12973);
#162=CONTEXT_DEPENDENT_SHAPE_REPRESENTATION(#93,#12988);
#163=CONTEXT_DEPENDENT_SHAPE_REPRESENTATION(#94,#12989);
#164=CONTEXT_DEPENDENT_SHAPE_REPRESENTATION(#95,#12990);
#165=CONTEXT_DEPENDENT_SHAPE_REPRESENTATION(#96,#12991);
#166=CONTEXT_DEPENDENT_SHAPE_REPRESENTATION(#97,#12992);
#167=CONTEXT_DEPENDENT_SHAPE_REPRESENTATION(#98,#12993);
#168=CONTEXT_DEPENDENT_SHAPE_REPRESENTATION(#99,#12994);
#169=CONTEXT_DEPENDENT_SHAPE_REPRESENTATION(#100,#12995);
#170=CONTEXT_DEPENDENT_SHAPE_REPRESENTATION(#101,#12996);
#171=CONTEXT_DEPENDENT_SHAPE_REPRESENTATION(#102,#12997);
#172=CONTEXT_DEPENDENT_SHAPE_REPRESENTATION(#103,#12998);
#173=CONTEXT_DEPENDENT_SHAPE_REPRESENTATION(#104,#12999);
#174=CONTEXT_DEPENDENT_SHAPE_REPRESENTATION(#105,#13000);
#175=CONTEXT_DEPENDENT_SHAPE_REPRESENTATION(#106,#13001);
#176=CONTEXT_DEPENDENT_SHAPE_REPRESENTATION(#107,#13002);
#177=CONTEXT_DEPENDENT_SHAPE_REPRESENTATION(#108,#13003);
#178=CONTEXT_DEPENDENT_SHAPE_REPRESENTATION(#109,#13004);
#179=CONTEXT_DEPENDENT_SHAPE_REPRESENTATION(#110,#13005);
#180=CONTEXT_DEPENDENT_SHAPE_REPRESENTATION(#111,#13006);
#181=CONTEXT_DEPENDENT_SHAPE_REPRESENTATION(#112,#13007);
#182=CONTEXT_DEPENDENT_SHAPE_REPRESENTATION(#113,#13008);
#183=CONTEXT_DEPENDENT_SHAPE_REPRESENTATION(#114,#13009);
#184=CONTEXT_DEPENDENT_SHAPE_REPRESENTATION(#115,#13010);
#185=CONTEXT_DEPENDENT_SHAPE_REPRESENTATION(#116,#13011);
#186=CONTEXT_DEPENDENT_SHAPE_REPRESENTATION(#117,#13012);
#187=CONTEXT_DEPENDENT_SHAPE_REPRESENTATION(#118,#13013);
#188=CONTEXT_DEPENDENT_SHAPE_REPRESENTATION(#119,#13014);
#189=CONTEXT_DEPENDENT_SHAPE_REPRESENTATION(#120,#13015);
#190=CONTEXT_DEPENDENT_SHAPE_REPRESENTATION(#121,#13016);
#191=CONTEXT_DEPENDENT_SHAPE_REPRESENTATION(#122,#13017);
#192=CONTEXT_DEPENDENT_SHAPE_REPRESENTATION(#123,#13018);
#193=CONTEXT_DEPENDENT_SHAPE_REPRESENTATION(#124,#13019);
#194=CONTEXT_DEPENDENT_SHAPE_REPRESENTATION(#125,#13020);
#195=CONTEXT_DEPENDENT_SHAPE_REPRESENTATION(#126,#13021);
#196=CONTEXT_DEPENDENT_SHAPE_REPRESENTATION(#127,#13022);
#197=CONTEXT_DEPENDENT_SHAPE_REPRESENTATION(#128,#13023);
#198=CONTEXT_DEPENDENT_SHAPE_REPRESENTATION(#129,#13024);
#199=CONTEXT_DEPENDENT_SHAPE_REPRESENTATION(#130,#13025);
#200=CONTEXT_DEPENDENT_SHAPE_REPRESENTATION(#131,#13026);
#201=CONTEXT_DEPENDENT_SHAPE_REPRESENTATION(#132,#13027);
#202=CONTEXT_DEPENDENT_SHAPE_REPRESENTATION(#133,#13028);
#203=CONTEXT_DEPENDENT_SHAPE_REPRESENTATION(#134,#13029);
#204=CONTEXT_DEPENDENT_SHAPE_REPRESENTATION(#135,#13030);
#205=CONTEXT_DEPENDENT_SHAPE_REPRESENTATION(#136,#13031);
#206=CONTEXT_DEPENDENT_SHAPE_REPRESENTATION(#137,#13032);
#207=CONTEXT_DEPENDENT_SHAPE_REPRESENTATION(#138,#13033);
#208=CONTEXT_DEPENDENT_SHAPE_REPRESENTATION(#139,#13034);
#209=CONTEXT_DEPENDENT_SHAPE_REPRESENTATION(#140,#13035);
#210=CONTEXT_DEPENDENT_SHAPE_REPRESENTATION(#141,#13036);
#211=CONTEXT_DEPENDENT_SHAPE_REPRESENTATION(#142,#13037);
#212=CONTEXT_DEPENDENT_SHAPE_REPRESENTATION(#143,#13038);
#213=CONTEXT_DEPENDENT_SHAPE_REPRESENTATION(#144,#13039);
#214=CONTEXT_DEPENDENT_SHAPE_REPRESENTATION(#145,#13040);
#215=CONTEXT_DEPENDENT_SHAPE_REPRESENTATION(#146,#13041);
#216=CONTEXT_DEPENDENT_SHAPE_REPRESENTATION(#147,#13042);
#217=CONTEXT_DEPENDENT_SHAPE_REPRESENTATION(#148,#13043);
#218=CONTEXT_DEPENDENT_SHAPE_REPRESENTATION(#149,#13048);
#219=CONTEXT_DEPENDENT_SHAPE_REPRESENTATION(#150,#13049);
#220=CONTEXT_DEPENDENT_SHAPE_REPRESENTATION(#151,#13050);
#221=CONTEXT_DEPENDENT_SHAPE_REPRESENTATION(#152,#13051);
#222=CONTEXT_DEPENDENT_SHAPE_REPRESENTATION(#153,#13052);
#223=CONTEXT_DEPENDENT_SHAPE_REPRESENTATION(#154,#13053);
#224=NEXT_ASSEMBLY_USAGE_OCCURRENCE('Inner ring:1','Inner ring:1',
'Inner ring:1',#13111,#13112,'Inner ring:1');
#225=NEXT_ASSEMBLY_USAGE_OCCURRENCE('Outer ring:1','Outer ring:1',
'Outer ring:1',#13111,#13113,'Outer ring:1');
#226=NEXT_ASSEMBLY_USAGE_OCCURRENCE('Balls:1','Balls:1','Balls:1',#13111,
#13114,'Balls:1');
#227=NEXT_ASSEMBLY_USAGE_OCCURRENCE('Cage:1','Cage:1','Cage:1',#13111,#13115,
'Cage:1');
#228=NEXT_ASSEMBLY_USAGE_OCCURRENCE('Seals 2RS:1','Seals 2RS:1',
'Seals 2RS:1',#13111,#13116,'Seals 2RS:1');
#229=NEXT_ASSEMBLY_USAGE_OCCURRENCE('Steel sleeve:1','Steel sleeve:1',
'Steel sleeve:1',#13118,#13119,'Steel sleeve:1');
#230=NEXT_ASSEMBLY_USAGE_OCCURRENCE('Ball retainer (plastic):1',
'Ball retainer (plastic):1','Ball retainer (plastic):1',#13118,#13120,
'Ball retainer (plastic):1');
#231=NEXT_ASSEMBLY_USAGE_OCCURRENCE('Base:1','Base:1','Base:1',#13098,#13099,
'Base:1');
#232=NEXT_ASSEMBLY_USAGE_OCCURRENCE('Foot:1','Foot:1','Foot:1',#13098,#13100,
'Foot:1');
#233=NEXT_ASSEMBLY_USAGE_OCCURRENCE('Foot (1):1','Foot (1):1',
'Foot (1):1',#13098,#13101,'Foot (1):1');
#234=NEXT_ASSEMBLY_USAGE_OCCURRENCE('Camshaft bearing post:1',
'Camshaft bearing post:1','Camshaft bearing post:1',#13098,#13102,
'Camshaft bearing post:1');
#235=NEXT_ASSEMBLY_USAGE_OCCURRENCE('Bearing cap:1','Bearing cap:1',
'Bearing cap:1',#13098,#13103,'Bearing cap:1');
#236=NEXT_ASSEMBLY_USAGE_OCCURRENCE('Bearing cap (1):1',
'Bearing cap (1):1','Bearing cap (1):1',#13098,#13104,
'Bearing cap (1):1');
#237=NEXT_ASSEMBLY_USAGE_OCCURRENCE('Camshaft bearing post (1):1',
'Camshaft bearing post (1):1','Camshaft bearing post (1):1',#13098,#13105,
'Camshaft bearing post (1):1');
#238=NEXT_ASSEMBLY_USAGE_OCCURRENCE('Bearing cap (2):1',
'Bearing cap (2):1','Bearing cap (2):1',#13098,#13106,
'Bearing cap (2):1');
#239=NEXT_ASSEMBLY_USAGE_OCCURRENCE('Bearing cap (3):1',
'Bearing cap (3):1','Bearing cap (3):1',#13098,#13107,
'Bearing cap (3):1');
#240=NEXT_ASSEMBLY_USAGE_OCCURRENCE('Valve guide bridge:1',
'Valve guide bridge:1','Valve guide bridge:1',#13098,#13108,
'Valve guide bridge:1');
#241=NEXT_ASSEMBLY_USAGE_OCCURRENCE('Stem guide cap:1',
'Stem guide cap:1','Stem guide cap:1',#13098,#13109,'Stem guide cap:1');
#242=NEXT_ASSEMBLY_USAGE_OCCURRENCE('Installed return spring:1',
'Installed return spring:1','Installed return spring:1',#13098,#13110,
'Installed return spring:1');
#243=NEXT_ASSEMBLY_USAGE_OCCURRENCE('Cap Screw - M4x16:2',
'Cap Screw - M4x16:2','Cap Screw - M4x16:2',#13098,#13134,
'Cap Screw - M4x16:2');
#244=NEXT_ASSEMBLY_USAGE_OCCURRENCE('Cap Screw - M4x16:3',
'Cap Screw - M4x16:3','Cap Screw - M4x16:3',#13098,#13134,
'Cap Screw - M4x16:3');
#245=NEXT_ASSEMBLY_USAGE_OCCURRENCE(
'Sealed Ball Bearing - 12 x 32 x 10 mm:2',
'Sealed Ball Bearing - 12 x 32 x 10 mm:2',
'Sealed Ball Bearing - 12 x 32 x 10 mm:2',#13098,#13111,
'Sealed Ball Bearing - 12 x 32 x 10 mm:2');
#246=NEXT_ASSEMBLY_USAGE_OCCURRENCE('M4x10 Cap Screw:2',
'M4x10 Cap Screw:2','M4x10 Cap Screw:2',#13098,#13121,
'M4x10 Cap Screw:2');
#247=NEXT_ASSEMBLY_USAGE_OCCURRENCE('M4x10 Cap Screw:3',
'M4x10 Cap Screw:3','M4x10 Cap Screw:3',#13098,#13121,
'M4x10 Cap Screw:3');
#248=NEXT_ASSEMBLY_USAGE_OCCURRENCE('M4x10 Cap Screw:4',
'M4x10 Cap Screw:4','M4x10 Cap Screw:4',#13098,#13121,
'M4x10 Cap Screw:4');
#249=NEXT_ASSEMBLY_USAGE_OCCURRENCE('M4x10 Cap Screw:5',
'M4x10 Cap Screw:5','M4x10 Cap Screw:5',#13098,#13121,
'M4x10 Cap Screw:5');
#250=NEXT_ASSEMBLY_USAGE_OCCURRENCE('M4x10 Cap Screw:6',
'M4x10 Cap Screw:6','M4x10 Cap Screw:6',#13098,#13121,
'M4x10 Cap Screw:6');
#251=NEXT_ASSEMBLY_USAGE_OCCURRENCE('M4x10 Cap Screw:7',
'M4x10 Cap Screw:7','M4x10 Cap Screw:7',#13098,#13121,
'M4x10 Cap Screw:7');
#252=NEXT_ASSEMBLY_USAGE_OCCURRENCE('M4x10 Cap Screw:8',
'M4x10 Cap Screw:8','M4x10 Cap Screw:8',#13098,#13121,
'M4x10 Cap Screw:8');
#253=NEXT_ASSEMBLY_USAGE_OCCURRENCE('M4x10 Cap Screw:9',
'M4x10 Cap Screw:9','M4x10 Cap Screw:9',#13098,#13121,
'M4x10 Cap Screw:9');
#254=NEXT_ASSEMBLY_USAGE_OCCURRENCE('Cap Screw - M4x16:4',
'Cap Screw - M4x16:4','Cap Screw - M4x16:4',#13098,#13134,
'Cap Screw - M4x16:4');
#255=NEXT_ASSEMBLY_USAGE_OCCURRENCE('Cap Screw - M4x16:5',
'Cap Screw - M4x16:5','Cap Screw - M4x16:5',#13098,#13134,
'Cap Screw - M4x16:5');
#256=NEXT_ASSEMBLY_USAGE_OCCURRENCE(
'Sealed Ball Bearing - 12 x 32 x 10 mm:3',
'Sealed Ball Bearing - 12 x 32 x 10 mm:3',
'Sealed Ball Bearing - 12 x 32 x 10 mm:3',#13098,#13111,
'Sealed Ball Bearing - 12 x 32 x 10 mm:3');
#257=NEXT_ASSEMBLY_USAGE_OCCURRENCE('M4x10 Cap Screw:10',
'M4x10 Cap Screw:10','M4x10 Cap Screw:10',#13098,#13121,
'M4x10 Cap Screw:10');
#258=NEXT_ASSEMBLY_USAGE_OCCURRENCE('M4x10 Cap Screw:11',
'M4x10 Cap Screw:11','M4x10 Cap Screw:11',#13098,#13121,
'M4x10 Cap Screw:11');
#259=NEXT_ASSEMBLY_USAGE_OCCURRENCE('M4x10 Cap Screw:12',
'M4x10 Cap Screw:12','M4x10 Cap Screw:12',#13098,#13121,
'M4x10 Cap Screw:12');
#260=NEXT_ASSEMBLY_USAGE_OCCURRENCE('M4x10 Cap Screw:13',
'M4x10 Cap Screw:13','M4x10 Cap Screw:13',#13098,#13121,
'M4x10 Cap Screw:13');
#261=NEXT_ASSEMBLY_USAGE_OCCURRENCE('M4x10 Cap Screw:14',
'M4x10 Cap Screw:14','M4x10 Cap Screw:14',#13098,#13121,
'M4x10 Cap Screw:14');
#262=NEXT_ASSEMBLY_USAGE_OCCURRENCE('M4x10 Cap Screw:15',
'M4x10 Cap Screw:15','M4x10 Cap Screw:15',#13098,#13121,
'M4x10 Cap Screw:15');
#263=NEXT_ASSEMBLY_USAGE_OCCURRENCE('M4x10 Cap Screw:16',
'M4x10 Cap Screw:16','M4x10 Cap Screw:16',#13098,#13121,
'M4x10 Cap Screw:16');
#264=NEXT_ASSEMBLY_USAGE_OCCURRENCE('M4x10 Cap Screw:17',
'M4x10 Cap Screw:17','M4x10 Cap Screw:17',#13098,#13121,
'M4x10 Cap Screw:17');
#265=NEXT_ASSEMBLY_USAGE_OCCURRENCE('Cap Screw - M5x20:2',
'Cap Screw - M5x20:2','Cap Screw - M5x20:2',#13098,#13117,
'Cap Screw - M5x20:2');
#266=NEXT_ASSEMBLY_USAGE_OCCURRENCE('Cap Screw - M5x20:3',
'Cap Screw - M5x20:3','Cap Screw - M5x20:3',#13098,#13117,
'Cap Screw - M5x20:3');
#267=NEXT_ASSEMBLY_USAGE_OCCURRENCE(
'Linear Ball Bushing - 12 x 21 x 30 mm:2',
'Linear Ball Bushing - 12 x 21 x 30 mm:2',
'Linear Ball Bushing - 12 x 21 x 30 mm:2',#13098,#13118,
'Linear Ball Bushing - 12 x 21 x 30 mm:2');
#268=NEXT_ASSEMBLY_USAGE_OCCURRENCE('M4x10 Cap Screw:18',
'M4x10 Cap Screw:18','M4x10 Cap Screw:18',#13098,#13121,
'M4x10 Cap Screw:18');
#269=NEXT_ASSEMBLY_USAGE_OCCURRENCE('M4x10 Cap Screw:19',
'M4x10 Cap Screw:19','M4x10 Cap Screw:19',#13098,#13121,
'M4x10 Cap Screw:19');
#270=NEXT_ASSEMBLY_USAGE_OCCURRENCE('M4x10 Cap Screw:20',
'M4x10 Cap Screw:20','M4x10 Cap Screw:20',#13098,#13121,
'M4x10 Cap Screw:20');
#271=NEXT_ASSEMBLY_USAGE_OCCURRENCE('M4x10 Cap Screw:21',
'M4x10 Cap Screw:21','M4x10 Cap Screw:21',#13098,#13121,
'M4x10 Cap Screw:21');
#272=NEXT_ASSEMBLY_USAGE_OCCURRENCE('Camshaft:1','Camshaft:1',
'Camshaft:1',#13122,#13123,'Camshaft:1');
#273=NEXT_ASSEMBLY_USAGE_OCCURRENCE('Inner race sleeve 10 mm:1',
'Inner race sleeve 10 mm:1','Inner race sleeve 10 mm:1',#13122,#13124,
'Inner race sleeve 10 mm:1');
#274=NEXT_ASSEMBLY_USAGE_OCCURRENCE('Inner race sleeve 10 mm (1):1',
'Inner race sleeve 10 mm (1):1','Inner race sleeve 10 mm (1):1',#13122,
#13125,'Inner race sleeve 10 mm (1):1');
#275=NEXT_ASSEMBLY_USAGE_OCCURRENCE('Inner race sleeve 15 mm:1',
'Inner race sleeve 15 mm:1','Inner race sleeve 15 mm:1',#13122,#13126,
'Inner race sleeve 15 mm:1');
#276=NEXT_ASSEMBLY_USAGE_OCCURRENCE('Inner race sleeve 15 mm (1):1',
'Inner race sleeve 15 mm (1):1','Inner race sleeve 15 mm (1):1',#13122,
#13127,'Inner race sleeve 15 mm (1):1');
#277=NEXT_ASSEMBLY_USAGE_OCCURRENCE('Eccentric cam:1','Eccentric cam:1',
'Eccentric cam:1',#13122,#13128,'Eccentric cam:1');
#278=NEXT_ASSEMBLY_USAGE_OCCURRENCE('Hand crank:1','Hand crank:1',
'Hand crank:1',#13122,#13129,'Hand crank:1');
#279=NEXT_ASSEMBLY_USAGE_OCCURRENCE('Crank grip:1','Crank grip:1',
'Crank grip:1',#13122,#13130,'Crank grip:1');
#280=NEXT_ASSEMBLY_USAGE_OCCURRENCE('Axial keeper:1','Axial keeper:1',
'Axial keeper:1',#13122,#13131,'Axial keeper:1');
#281=NEXT_ASSEMBLY_USAGE_OCCURRENCE('Axial keeper (1):1',
'Axial keeper (1):1','Axial keeper (1):1',#13122,#13132,
'Axial keeper (1):1');
#282=NEXT_ASSEMBLY_USAGE_OCCURRENCE('Key 4x4x14:2','Key 4x4x14:2',
'Key 4x4x14:2',#13122,#13133,'Key 4x4x14:2');
#283=NEXT_ASSEMBLY_USAGE_OCCURRENCE('Key 4x4x14:3','Key 4x4x14:3',
'Key 4x4x14:3',#13122,#13133,'Key 4x4x14:3');
#284=NEXT_ASSEMBLY_USAGE_OCCURRENCE('Cap Screw - M4x16:6',
'Cap Screw - M4x16:6','Cap Screw - M4x16:6',#13122,#13134,
'Cap Screw - M4x16:6');
#285=NEXT_ASSEMBLY_USAGE_OCCURRENCE('Cap Screw - M4x16:7',
'Cap Screw - M4x16:7','Cap Screw - M4x16:7',#13122,#13134,
'Cap Screw - M4x16:7');
#286=NEXT_ASSEMBLY_USAGE_OCCURRENCE('Cap Screw - M4x16:8',
'Cap Screw - M4x16:8','Cap Screw - M4x16:8',#13122,#13134,
'Cap Screw - M4x16:8');
#287=NEXT_ASSEMBLY_USAGE_OCCURRENCE('Flat follower shoe:1',
'Flat follower shoe:1','Flat follower shoe:1',#13135,#13136,
'Flat follower shoe:1');
#288=NEXT_ASSEMBLY_USAGE_OCCURRENCE('Valve stem:1','Valve stem:1',
'Valve stem:1',#13135,#13137,'Valve stem:1');
#289=NEXT_ASSEMBLY_USAGE_OCCURRENCE('Spring seat washer:1',
'Spring seat washer:1','Spring seat washer:1',#13135,#13138,
'Spring seat washer:1');
#290=NEXT_ASSEMBLY_USAGE_OCCURRENCE('Bearing frame and stem guide:1',
'Bearing frame and stem guide:1','Bearing frame and stem guide:1',#13097,
#13098,'Bearing frame and stem guide:1');
#291=NEXT_ASSEMBLY_USAGE_OCCURRENCE('Camshaft and hand crank:1',
'Camshaft and hand crank:1','Camshaft and hand crank:1',#13097,#13122,
'Camshaft and hand crank:1');
#292=NEXT_ASSEMBLY_USAGE_OCCURRENCE('Valve stem and follower:1',
'Valve stem and follower:1','Valve stem and follower:1',#13097,#13135,
'Valve stem and follower:1');
#293=SPHERICAL_SURFACE('',#6956,0.29765);
#294=SPHERICAL_SURFACE('',#6958,0.29765);
#295=SPHERICAL_SURFACE('',#6960,0.29765);
#296=SPHERICAL_SURFACE('',#6962,0.29765);
#297=SPHERICAL_SURFACE('',#6964,0.29765);
#298=SPHERICAL_SURFACE('',#6966,0.29765);
#299=SPHERICAL_SURFACE('',#6968,0.29765);
#300=SPHERICAL_SURFACE('',#6971,0.309556);
#301=SPHERICAL_SURFACE('',#6987,0.309556);
#302=SPHERICAL_SURFACE('',#6992,0.309556);
#303=SPHERICAL_SURFACE('',#6998,0.309556);
#304=SPHERICAL_SURFACE('',#7003,0.309556);
#305=SPHERICAL_SURFACE('',#7008,0.309556);
#306=SPHERICAL_SURFACE('',#7016,0.309556);
#307=CONICAL_SURFACE('',#6927,0.63,0.785398163397448);
#308=CONICAL_SURFACE('',#6934,0.63,0.785398163397448);
#309=CONICAL_SURFACE('',#6947,1.57,0.785398163397449);
#310=CONICAL_SURFACE('',#6951,1.57,0.785398163397449);
#311=CONICAL_SURFACE('',#7045,0.4,0.785398163397448);
#312=CONICAL_SURFACE('',#7049,0.41,0.785398163397448);
#313=CONICAL_SURFACE('',#7053,0.26,0.463647609000806);
#314=CONICAL_SURFACE('',#7057,0.225,0.785398163397448);
#315=CONICAL_SURFACE('',#7133,0.325,0.785398163397448);
#316=CONICAL_SURFACE('',#7137,0.335,0.785398163397448);
#317=CONICAL_SURFACE('',#7141,0.21,0.463647609000806);
#318=CONICAL_SURFACE('',#7295,0.325,0.785398163397448);
#319=CONICAL_SURFACE('',#7299,0.335,0.785398163397448);
#320=CONICAL_SURFACE('',#7303,0.21,0.463647609000806);
#321=CONICAL_SURFACE('',#7307,0.18,0.785398163397448);
#322=TOROIDAL_SURFACE('',#6916,1.1,0.309556);
#323=TOROIDAL_SURFACE('',#6936,1.1,0.309556);
#324=B_SPLINE_CURVE_WITH_KNOTS('',3,(#11366,#11367,#11368,#11369,#11370,
#11371,#11372,#11373,#11374,#11375,#11376,#11377,#11378,#11379,#11380,#11381,
#11382,#11383,#11384,#11385,#11386,#11387,#11388,#11389,#11390,#11391,#11392,
#11393,#11394,#11395,#11396,#11397,#11398,#11399,#11400,#11401,#11402,#11403,
#11404,#11405,#11406,#11407,#11408,#11409,#11410,#11411,#11412,#11413,#11414,
#11415,#11416,#11417,#11418,#11419,#11420,#11421,#11422,#11423,#11424,#11425,
#11426,#11427,#11428,#11429,#11430,#11431,#11432,#11433,#11434,#11435,#11436,
#11437,#11438,#11439,#11440,#11441,#11442,#11443,#11444,#11445,#11446,#11447,
#11448,#11449,#11450,#11451,#11452,#11453,#11454,#11455,#11456,#11457,#11458,
#11459,#11460,#11461,#11462,#11463,#11464,#11465,#11466,#11467,#11468,#11469,
#11470,#11471,#11472,#11473,#11474,#11475,#11476,#11477,#11478,#11479,#11480,
#11481,#11482,#11483,#11484,#11485,#11486,#11487,#11488,#11489),
 .UNSPECIFIED.,.F.,.F.,(4,1,1,1,1,1,1,1,1,1,1,1,1,1,1,1,1,1,1,1,1,1,1,1,
1,1,1,1,1,1,1,1,1,1,1,1,1,1,1,1,1,1,1,1,1,1,1,1,1,1,1,1,1,1,1,1,1,1,1,1,
1,1,1,1,1,1,1,1,1,1,1,1,1,1,1,1,1,1,1,1,1,1,1,1,1,1,1,1,1,1,1,1,1,1,1,1,
1,1,1,1,1,1,1,1,1,1,1,1,1,1,1,1,1,1,1,1,1,1,1,1,1,4),(0.,0.00892857142857143,
0.0178571428571429,0.0267857142857143,0.0357142857142857,0.0446428571428571,
0.0535714285714286,0.0625,0.0714285714285714,0.0803571428571428,0.0892857142857143,
0.0982142857142857,0.107142857142857,0.116071428571429,0.125,0.133928571428571,
0.142857142857143,0.150793650793651,0.158730158730159,0.166666666666667,
0.174603174603175,0.182539682539683,0.19047619047619,0.202380952380952,
0.214285714285714,0.222222222222222,0.23015873015873,0.238095238095238,
0.244047619047619,0.25,0.255952380952381,0.261904761904762,0.273809523809524,
0.285714285714286,0.297619047619048,0.30952380952381,0.321428571428571,
0.333333333333333,0.341269841269841,0.349206349206349,0.357142857142857,
0.365079365079365,0.373015873015873,0.375,0.376984126984127,0.380952380952381,
0.386904761904762,0.392857142857143,0.404761904761905,0.416666666666667,
0.428571428571429,0.4375,0.446428571428571,0.455357142857143,0.464285714285714,
0.468253968253968,0.476190476190476,0.482142857142857,0.488095238095238,
0.494047619047619,0.5,0.508928571428571,0.517857142857143,0.526785714285714,
0.535714285714286,0.544642857142857,0.553571428571429,0.5625,0.571428571428571,
0.580357142857143,0.589285714285714,0.598214285714286,0.607142857142857,
0.616071428571429,0.625,0.633928571428571,0.642857142857143,0.650793650793651,
0.658730158730159,0.666666666666667,0.672619047619048,0.678571428571428,
0.69047619047619,0.696428571428571,0.702380952380952,0.714285714285714,
0.726190476190476,0.732142857142857,0.738095238095238,0.746031746031746,
0.753968253968254,0.761904761904762,0.76984126984127,0.777777777777778,
0.785714285714286,0.787946428571428,0.790178571428571,0.794642857142857,
0.803571428571428,0.808035714285714,0.8125,0.821428571428571,0.830357142857143,
0.839285714285714,0.848214285714286,0.857142857142857,0.866071428571429,
0.875,0.883928571428571,0.892857142857143,0.901785714285714,0.910714285714286,
0.919642857142857,0.928571428571429,0.9375,0.946428571428571,0.955357142857143,
0.964285714285714,0.973214285714286,0.982142857142857,0.991071428571429,
1.),.UNSPECIFIED.);
#325=B_SPLINE_CURVE_WITH_KNOTS('',3,(#11597,#11598,#11599,#11600,#11601,
#11602,#11603,#11604,#11605,#11606,#11607,#11608,#11609,#11610,#11611,#11612,
#11613,#11614,#11615,#11616,#11617,#11618),.UNSPECIFIED.,.F.,.F.,(4,2,2,
2,2,2,2,2,2,2,4),(0.0591825211272536,0.157966726598481,0.236950089897721,
0.315933453196962,0.391576304923761,0.46721915665056,0.54286200837736,0.618504860104159,
0.697488223403399,0.77647158670264,0.875255792173867),.UNSPECIFIED.);
#326=B_SPLINE_CURVE_WITH_KNOTS('',3,(#11622,#11623,#11624,#11625,#11626,
#11627,#11628,#11629,#11630,#11631,#11632,#11633,#11634,#11635,#11636,#11637,
#11638,#11639,#11640,#11641,#11642,#11643),.UNSPECIFIED.,.F.,.F.,(4,2,2,
2,2,2,2,2,2,2,4),(0.0581119756758434,0.106553146291161,0.213106292582322,
0.30849933801665,0.386091982889075,0.4636846277615,0.541277272633925,0.61886991750635,
0.714262962940678,0.820816109231839,0.869257279847157),.UNSPECIFIED.);
#327=B_SPLINE_CURVE_WITH_KNOTS('',3,(#11649,#11650,#11651,#11652,#11653,
#11654,#11655,#11656,#11657,#11658,#11659,#11660,#11661,#11662,#11663,#11664,
#11665,#11666,#11667,#11668,#11669,#11670),.UNSPECIFIED.,.F.,.F.,(4,2,2,
2,2,2,2,2,2,2,4),(0.0581119756758434,0.106553146291161,0.213106292582322,
0.30849933801665,0.386091982889075,0.4636846277615,0.541277272633925,0.61886991750635,
0.714262962940679,0.820816109231839,0.869257279847157),.UNSPECIFIED.);
#328=B_SPLINE_CURVE_WITH_KNOTS('',3,(#11674,#11675,#11676,#11677,#11678,
#11679,#11680,#11681,#11682,#11683,#11684,#11685,#11686,#11687,#11688,#11689,
#11690,#11691,#11692,#11693,#11694,#11695),.UNSPECIFIED.,.F.,.F.,(4,2,2,
2,2,2,2,2,2,2,4),(0.0581119756758433,0.106553146291161,0.213106292582322,
0.308499338016649,0.386091982889075,0.4636846277615,0.541277272633925,0.61886991750635,
0.714262962940678,0.820816109231839,0.869257279847157),.UNSPECIFIED.);
#329=B_SPLINE_CURVE_WITH_KNOTS('',3,(#11704,#11705,#11706,#11707,#11708,
#11709,#11710,#11711,#11712,#11713,#11714,#11715,#11716,#11717,#11718,#11719,
#11720,#11721,#11722,#11723,#11724,#11725),.UNSPECIFIED.,.F.,.F.,(4,2,2,
2,2,2,2,2,2,2,4),(0.0581119756758433,0.106553146291161,0.213106292582322,
0.30849933801665,0.386091982889075,0.4636846277615,0.541277272633925,0.61886991750635,
0.714262962940678,0.820816109231839,0.869257279847157),.UNSPECIFIED.);
#330=B_SPLINE_CURVE_WITH_KNOTS('',3,(#11729,#11730,#11731,#11732,#11733,
#11734,#11735,#11736,#11737,#11738,#11739,#11740,#11741,#11742,#11743,#11744,
#11745,#11746,#11747,#11748,#11749,#11750),.UNSPECIFIED.,.F.,.F.,(4,2,2,
2,2,2,2,2,2,2,4),(0.0581119756758434,0.106553146291161,0.213106292582322,
0.30849933801665,0.386091982889075,0.4636846277615,0.541277272633925,0.61886991750635,
0.714262962940678,0.820816109231839,0.869257279847157),.UNSPECIFIED.);
#331=B_SPLINE_CURVE_WITH_KNOTS('',3,(#11754,#11755,#11756,#11757,#11758,
#11759,#11760,#11761,#11762,#11763,#11764,#11765,#11766,#11767,#11768,#11769,
#11770,#11771,#11772,#11773,#11774,#11775),.UNSPECIFIED.,.F.,.F.,(4,2,2,
2,2,2,2,2,2,2,4),(0.0581119756758434,0.106553146291161,0.213106292582322,
0.30849933801665,0.386091982889075,0.4636846277615,0.541277272633925,0.61886991750635,
0.714262962940678,0.820816109231839,0.869257279847157),.UNSPECIFIED.);
#332=B_SPLINE_CURVE_WITH_KNOTS('',3,(#11779,#11780,#11781,#11782,#11783,
#11784,#11785,#11786,#11787,#11788,#11789,#11790,#11791,#11792,#11793,#11794,
#11795,#11796,#11797,#11798,#11799,#11800),.UNSPECIFIED.,.F.,.F.,(4,2,2,
2,2,2,2,2,2,2,4),(0.0581119756758433,0.106553146291161,0.213106292582322,
0.30849933801665,0.386091982889075,0.4636846277615,0.541277272633925,0.61886991750635,
0.714262962940678,0.820816109231839,0.869257279847157),.UNSPECIFIED.);
#333=B_SPLINE_CURVE_WITH_KNOTS('',3,(#11808,#11809,#11810,#11811,#11812,
#11813,#11814,#11815,#11816,#11817,#11818,#11819,#11820,#11821,#11822,#11823,
#11824,#11825,#11826,#11827,#11828,#11829),.UNSPECIFIED.,.F.,.F.,(4,2,2,
2,2,2,2,2,2,2,4),(0.0591825211272536,0.157966726598481,0.236950089897721,
0.315933453196962,0.391576304923761,0.467219156650561,0.54286200837736,
0.618504860104159,0.697488223403399,0.77647158670264,0.875255792173867),
 .UNSPECIFIED.);
#334=B_SPLINE_CURVE_WITH_KNOTS('',3,(#11837,#11838,#11839,#11840,#11841,
#11842,#11843,#11844,#11845,#11846,#11847,#11848,#11849,#11850,#11851,#11852,
#11853,#11854,#11855,#11856,#11857,#11858),.UNSPECIFIED.,.F.,.F.,(4,2,2,
2,2,2,2,2,2,2,4),(0.0591825211272536,0.157966726598481,0.236950089897722,
0.315933453196962,0.391576304923761,0.467219156650561,0.54286200837736,
0.618504860104159,0.697488223403399,0.77647158670264,0.875255792173867),
 .UNSPECIFIED.);
#335=B_SPLINE_CURVE_WITH_KNOTS('',3,(#11868,#11869,#11870,#11871,#11872,
#11873,#11874,#11875,#11876,#11877,#11878,#11879,#11880,#11881,#11882,#11883,
#11884,#11885,#11886,#11887,#11888,#11889),.UNSPECIFIED.,.F.,.F.,(4,2,2,
2,2,2,2,2,2,2,4),(0.0591825211272536,0.157966726598481,0.236950089897721,
0.315933453196962,0.391576304923761,0.46721915665056,0.54286200837736,0.618504860104159,
0.697488223403399,0.77647158670264,0.875255792173867),.UNSPECIFIED.);
#336=B_SPLINE_CURVE_WITH_KNOTS('',3,(#11897,#11898,#11899,#11900,#11901,
#11902,#11903,#11904,#11905,#11906,#11907,#11908,#11909,#11910,#11911,#11912,
#11913,#11914,#11915,#11916,#11917,#11918),.UNSPECIFIED.,.F.,.F.,(4,2,2,
2,2,2,2,2,2,2,4),(0.0591825211272536,0.157966726598481,0.236950089897721,
0.315933453196962,0.391576304923761,0.46721915665056,0.542862008377359,
0.618504860104159,0.697488223403399,0.776471586702639,0.875255792173867),
 .UNSPECIFIED.);
#337=B_SPLINE_CURVE_WITH_KNOTS('',3,(#11926,#11927,#11928,#11929,#11930,
#11931,#11932,#11933,#11934,#11935,#11936,#11937,#11938,#11939,#11940,#11941,
#11942,#11943,#11944,#11945,#11946,#11947),.UNSPECIFIED.,.F.,.F.,(4,2,2,
2,2,2,2,2,2,2,4),(0.0591825211272536,0.157966726598481,0.236950089897721,
0.315933453196962,0.391576304923761,0.46721915665056,0.54286200837736,0.618504860104159,
0.697488223403399,0.77647158670264,0.875255792173867),.UNSPECIFIED.);
#338=B_SPLINE_CURVE_WITH_KNOTS('',3,(#11956,#11957,#11958,#11959,#11960,
#11961,#11962,#11963,#11964,#11965,#11966,#11967,#11968,#11969,#11970,#11971,
#11972,#11973,#11974,#11975,#11976,#11977),.UNSPECIFIED.,.F.,.F.,(4,2,2,
2,2,2,2,2,2,2,4),(0.0591825211272536,0.157966726598481,0.236950089897721,
0.315933453196962,0.391576304923761,0.46721915665056,0.542862008377359,
0.618504860104159,0.697488223403399,0.776471586702639,0.875255792173867),
 .UNSPECIFIED.);
#339=B_SPLINE_SURFACE_WITH_KNOTS('',3,3,((#10123,#10124,#10125,#10126,#10127,
#10128,#10129,#10130,#10131,#10132,#10133,#10134,#10135,#10136,#10137,#10138,
#10139,#10140,#10141,#10142,#10143,#10144,#10145,#10146,#10147,#10148,#10149,
#10150,#10151,#10152,#10153,#10154,#10155,#10156,#10157,#10158,#10159,#10160,
#10161,#10162,#10163,#10164,#10165,#10166,#10167,#10168,#10169,#10170,#10171,
#10172,#10173,#10174,#10175,#10176,#10177,#10178,#10179,#10180,#10181,#10182,
#10183,#10184,#10185,#10186,#10187,#10188,#10189,#10190,#10191,#10192,#10193,
#10194,#10195,#10196,#10197,#10198,#10199,#10200,#10201,#10202,#10203,#10204,
#10205,#10206,#10207,#10208,#10209,#10210,#10211,#10212,#10213,#10214,#10215,
#10216,#10217,#10218,#10219,#10220,#10221,#10222,#10223,#10224,#10225,#10226,
#10227,#10228,#10229,#10230,#10231,#10232,#10233,#10234,#10235,#10236,#10237,
#10238,#10239,#10240,#10241,#10242,#10243,#10244,#10245,#10246),(#10247,
#10248,#10249,#10250,#10251,#10252,#10253,#10254,#10255,#10256,#10257,#10258,
#10259,#10260,#10261,#10262,#10263,#10264,#10265,#10266,#10267,#10268,#10269,
#10270,#10271,#10272,#10273,#10274,#10275,#10276,#10277,#10278,#10279,#10280,
#10281,#10282,#10283,#10284,#10285,#10286,#10287,#10288,#10289,#10290,#10291,
#10292,#10293,#10294,#10295,#10296,#10297,#10298,#10299,#10300,#10301,#10302,
#10303,#10304,#10305,#10306,#10307,#10308,#10309,#10310,#10311,#10312,#10313,
#10314,#10315,#10316,#10317,#10318,#10319,#10320,#10321,#10322,#10323,#10324,
#10325,#10326,#10327,#10328,#10329,#10330,#10331,#10332,#10333,#10334,#10335,
#10336,#10337,#10338,#10339,#10340,#10341,#10342,#10343,#10344,#10345,#10346,
#10347,#10348,#10349,#10350,#10351,#10352,#10353,#10354,#10355,#10356,#10357,
#10358,#10359,#10360,#10361,#10362,#10363,#10364,#10365,#10366,#10367,#10368,
#10369,#10370),(#10371,#10372,#10373,#10374,#10375,#10376,#10377,#10378,
#10379,#10380,#10381,#10382,#10383,#10384,#10385,#10386,#10387,#10388,#10389,
#10390,#10391,#10392,#10393,#10394,#10395,#10396,#10397,#10398,#10399,#10400,
#10401,#10402,#10403,#10404,#10405,#10406,#10407,#10408,#10409,#10410,#10411,
#10412,#10413,#10414,#10415,#10416,#10417,#10418,#10419,#10420,#10421,#10422,
#10423,#10424,#10425,#10426,#10427,#10428,#10429,#10430,#10431,#10432,#10433,
#10434,#10435,#10436,#10437,#10438,#10439,#10440,#10441,#10442,#10443,#10444,
#10445,#10446,#10447,#10448,#10449,#10450,#10451,#10452,#10453,#10454,#10455,
#10456,#10457,#10458,#10459,#10460,#10461,#10462,#10463,#10464,#10465,#10466,
#10467,#10468,#10469,#10470,#10471,#10472,#10473,#10474,#10475,#10476,#10477,
#10478,#10479,#10480,#10481,#10482,#10483,#10484,#10485,#10486,#10487,#10488,
#10489,#10490,#10491,#10492,#10493,#10494),(#10495,#10496,#10497,#10498,
#10499,#10500,#10501,#10502,#10503,#10504,#10505,#10506,#10507,#10508,#10509,
#10510,#10511,#10512,#10513,#10514,#10515,#10516,#10517,#10518,#10519,#10520,
#10521,#10522,#10523,#10524,#10525,#10526,#10527,#10528,#10529,#10530,#10531,
#10532,#10533,#10534,#10535,#10536,#10537,#10538,#10539,#10540,#10541,#10542,
#10543,#10544,#10545,#10546,#10547,#10548,#10549,#10550,#10551,#10552,#10553,
#10554,#10555,#10556,#10557,#10558,#10559,#10560,#10561,#10562,#10563,#10564,
#10565,#10566,#10567,#10568,#10569,#10570,#10571,#10572,#10573,#10574,#10575,
#10576,#10577,#10578,#10579,#10580,#10581,#10582,#10583,#10584,#10585,#10586,
#10587,#10588,#10589,#10590,#10591,#10592,#10593,#10594,#10595,#10596,#10597,
#10598,#10599,#10600,#10601,#10602,#10603,#10604,#10605,#10606,#10607,#10608,
#10609,#10610,#10611,#10612,#10613,#10614,#10615,#10616,#10617,#10618),
(#10619,#10620,#10621,#10622,#10623,#10624,#10625,#10626,#10627,#10628,
#10629,#10630,#10631,#10632,#10633,#10634,#10635,#10636,#10637,#10638,#10639,
#10640,#10641,#10642,#10643,#10644,#10645,#10646,#10647,#10648,#10649,#10650,
#10651,#10652,#10653,#10654,#10655,#10656,#10657,#10658,#10659,#10660,#10661,
#10662,#10663,#10664,#10665,#10666,#10667,#10668,#10669,#10670,#10671,#10672,
#10673,#10674,#10675,#10676,#10677,#10678,#10679,#10680,#10681,#10682,#10683,
#10684,#10685,#10686,#10687,#10688,#10689,#10690,#10691,#10692,#10693,#10694,
#10695,#10696,#10697,#10698,#10699,#10700,#10701,#10702,#10703,#10704,#10705,
#10706,#10707,#10708,#10709,#10710,#10711,#10712,#10713,#10714,#10715,#10716,
#10717,#10718,#10719,#10720,#10721,#10722,#10723,#10724,#10725,#10726,#10727,
#10728,#10729,#10730,#10731,#10732,#10733,#10734,#10735,#10736,#10737,#10738,
#10739,#10740,#10741,#10742),(#10743,#10744,#10745,#10746,#10747,#10748,
#10749,#10750,#10751,#10752,#10753,#10754,#10755,#10756,#10757,#10758,#10759,
#10760,#10761,#10762,#10763,#10764,#10765,#10766,#10767,#10768,#10769,#10770,
#10771,#10772,#10773,#10774,#10775,#10776,#10777,#10778,#10779,#10780,#10781,
#10782,#10783,#10784,#10785,#10786,#10787,#10788,#10789,#10790,#10791,#10792,
#10793,#10794,#10795,#10796,#10797,#10798,#10799,#10800,#10801,#10802,#10803,
#10804,#10805,#10806,#10807,#10808,#10809,#10810,#10811,#10812,#10813,#10814,
#10815,#10816,#10817,#10818,#10819,#10820,#10821,#10822,#10823,#10824,#10825,
#10826,#10827,#10828,#10829,#10830,#10831,#10832,#10833,#10834,#10835,#10836,
#10837,#10838,#10839,#10840,#10841,#10842,#10843,#10844,#10845,#10846,#10847,
#10848,#10849,#10850,#10851,#10852,#10853,#10854,#10855,#10856,#10857,#10858,
#10859,#10860,#10861,#10862,#10863,#10864,#10865,#10866),(#10867,#10868,
#10869,#10870,#10871,#10872,#10873,#10874,#10875,#10876,#10877,#10878,#10879,
#10880,#10881,#10882,#10883,#10884,#10885,#10886,#10887,#10888,#10889,#10890,
#10891,#10892,#10893,#10894,#10895,#10896,#10897,#10898,#10899,#10900,#10901,
#10902,#10903,#10904,#10905,#10906,#10907,#10908,#10909,#10910,#10911,#10912,
#10913,#10914,#10915,#10916,#10917,#10918,#10919,#10920,#10921,#10922,#10923,
#10924,#10925,#10926,#10927,#10928,#10929,#10930,#10931,#10932,#10933,#10934,
#10935,#10936,#10937,#10938,#10939,#10940,#10941,#10942,#10943,#10944,#10945,
#10946,#10947,#10948,#10949,#10950,#10951,#10952,#10953,#10954,#10955,#10956,
#10957,#10958,#10959,#10960,#10961,#10962,#10963,#10964,#10965,#10966,#10967,
#10968,#10969,#10970,#10971,#10972,#10973,#10974,#10975,#10976,#10977,#10978,
#10979,#10980,#10981,#10982,#10983,#10984,#10985,#10986,#10987,#10988,#10989,
#10990),(#10991,#10992,#10993,#10994,#10995,#10996,#10997,#10998,#10999,
#11000,#11001,#11002,#11003,#11004,#11005,#11006,#11007,#11008,#11009,#11010,
#11011,#11012,#11013,#11014,#11015,#11016,#11017,#11018,#11019,#11020,#11021,
#11022,#11023,#11024,#11025,#11026,#11027,#11028,#11029,#11030,#11031,#11032,
#11033,#11034,#11035,#11036,#11037,#11038,#11039,#11040,#11041,#11042,#11043,
#11044,#11045,#11046,#11047,#11048,#11049,#11050,#11051,#11052,#11053,#11054,
#11055,#11056,#11057,#11058,#11059,#11060,#11061,#11062,#11063,#11064,#11065,
#11066,#11067,#11068,#11069,#11070,#11071,#11072,#11073,#11074,#11075,#11076,
#11077,#11078,#11079,#11080,#11081,#11082,#11083,#11084,#11085,#11086,#11087,
#11088,#11089,#11090,#11091,#11092,#11093,#11094,#11095,#11096,#11097,#11098,
#11099,#11100,#11101,#11102,#11103,#11104,#11105,#11106,#11107,#11108,#11109,
#11110,#11111,#11112,#11113,#11114),(#11115,#11116,#11117,#11118,#11119,
#11120,#11121,#11122,#11123,#11124,#11125,#11126,#11127,#11128,#11129,#11130,
#11131,#11132,#11133,#11134,#11135,#11136,#11137,#11138,#11139,#11140,#11141,
#11142,#11143,#11144,#11145,#11146,#11147,#11148,#11149,#11150,#11151,#11152,
#11153,#11154,#11155,#11156,#11157,#11158,#11159,#11160,#11161,#11162,#11163,
#11164,#11165,#11166,#11167,#11168,#11169,#11170,#11171,#11172,#11173,#11174,
#11175,#11176,#11177,#11178,#11179,#11180,#11181,#11182,#11183,#11184,#11185,
#11186,#11187,#11188,#11189,#11190,#11191,#11192,#11193,#11194,#11195,#11196,
#11197,#11198,#11199,#11200,#11201,#11202,#11203,#11204,#11205,#11206,#11207,
#11208,#11209,#11210,#11211,#11212,#11213,#11214,#11215,#11216,#11217,#11218,
#11219,#11220,#11221,#11222,#11223,#11224,#11225,#11226,#11227,#11228,#11229,
#11230,#11231,#11232,#11233,#11234,#11235,#11236,#11237,#11238),(#11239,
#11240,#11241,#11242,#11243,#11244,#11245,#11246,#11247,#11248,#11249,#11250,
#11251,#11252,#11253,#11254,#11255,#11256,#11257,#11258,#11259,#11260,#11261,
#11262,#11263,#11264,#11265,#11266,#11267,#11268,#11269,#11270,#11271,#11272,
#11273,#11274,#11275,#11276,#11277,#11278,#11279,#11280,#11281,#11282,#11283,
#11284,#11285,#11286,#11287,#11288,#11289,#11290,#11291,#11292,#11293,#11294,
#11295,#11296,#11297,#11298,#11299,#11300,#11301,#11302,#11303,#11304,#11305,
#11306,#11307,#11308,#11309,#11310,#11311,#11312,#11313,#11314,#11315,#11316,
#11317,#11318,#11319,#11320,#11321,#11322,#11323,#11324,#11325,#11326,#11327,
#11328,#11329,#11330,#11331,#11332,#11333,#11334,#11335,#11336,#11337,#11338,
#11339,#11340,#11341,#11342,#11343,#11344,#11345,#11346,#11347,#11348,#11349,
#11350,#11351,#11352,#11353,#11354,#11355,#11356,#11357,#11358,#11359,#11360,
#11361,#11362)),.UNSPECIFIED.,.T.,.F.,.F.,(4,1,1,1,1,1,1,4),(4,1,1,1,1,
1,1,1,1,1,1,1,1,1,1,1,1,1,1,1,1,1,1,1,1,1,1,1,1,1,1,1,1,1,1,1,1,1,1,1,1,
1,1,1,1,1,1,1,1,1,1,1,1,1,1,1,1,1,1,1,1,1,1,1,1,1,1,1,1,1,1,1,1,1,1,1,1,
1,1,1,1,1,1,1,1,1,1,1,1,1,1,1,1,1,1,1,1,1,1,1,1,1,1,1,1,1,1,1,1,1,1,1,1,
1,1,1,1,1,1,1,1,4),(-3.14159265358979,-2.24399475256414,-1.34639685153848,
-0.448798950512828,0.448798950512828,1.34639685153848,2.24399475256414,
3.14159265358979),(0.,0.00892857142857143,0.0178571428571429,0.0267857142857143,
0.0357142857142857,0.0446428571428571,0.0535714285714286,0.0625,0.0714285714285714,
0.0803571428571428,0.0892857142857143,0.0982142857142857,0.107142857142857,
0.116071428571429,0.125,0.133928571428571,0.142857142857143,0.150793650793651,
0.158730158730159,0.166666666666667,0.174603174603175,0.182539682539683,
0.19047619047619,0.202380952380952,0.214285714285714,0.222222222222222,
0.23015873015873,0.238095238095238,0.244047619047619,0.25,0.255952380952381,
0.261904761904762,0.273809523809524,0.285714285714286,0.297619047619048,
0.30952380952381,0.321428571428571,0.333333333333333,0.341269841269841,
0.349206349206349,0.357142857142857,0.365079365079365,0.373015873015873,
0.375,0.376984126984127,0.380952380952381,0.386904761904762,0.392857142857143,
0.404761904761905,0.416666666666667,0.428571428571429,0.4375,0.446428571428571,
0.455357142857143,0.464285714285714,0.468253968253968,0.476190476190476,
0.482142857142857,0.488095238095238,0.494047619047619,0.5,0.508928571428571,
0.517857142857143,0.526785714285714,0.535714285714286,0.544642857142857,
0.553571428571429,0.5625,0.571428571428571,0.580357142857143,0.589285714285714,
0.598214285714286,0.607142857142857,0.616071428571429,0.625,0.633928571428571,
0.642857142857143,0.650793650793651,0.658730158730159,0.666666666666667,
0.672619047619048,0.678571428571428,0.69047619047619,0.696428571428571,
0.702380952380952,0.714285714285714,0.726190476190476,0.732142857142857,
0.738095238095238,0.746031746031746,0.753968253968254,0.761904761904762,
0.76984126984127,0.777777777777778,0.785714285714286,0.787946428571428,
0.790178571428571,0.794642857142857,0.803571428571428,0.808035714285714,
0.8125,0.821428571428571,0.830357142857143,0.839285714285714,0.848214285714286,
0.857142857142857,0.866071428571429,0.875,0.883928571428571,0.892857142857143,
0.901785714285714,0.910714285714286,0.919642857142857,0.928571428571429,
0.9375,0.946428571428571,0.955357142857143,0.964285714285714,0.973214285714286,
0.982142857142857,0.991071428571429,1.),.UNSPECIFIED.);
#340=SHAPE_REPRESENTATION_RELATIONSHIP('SRR','None',#13056,#376);
#341=SHAPE_REPRESENTATION_RELATIONSHIP('SRR','None',#13057,#377);
#342=SHAPE_REPRESENTATION_RELATIONSHIP('SRR','None',#13058,#378);
#343=SHAPE_REPRESENTATION_RELATIONSHIP('SRR','None',#13059,#379);
#344=SHAPE_REPRESENTATION_RELATIONSHIP('SRR','None',#13060,#380);
#345=SHAPE_REPRESENTATION_RELATIONSHIP('SRR','None',#13061,#381);
#346=SHAPE_REPRESENTATION_RELATIONSHIP('SRR','None',#13062,#382);
#347=SHAPE_REPRESENTATION_RELATIONSHIP('SRR','None',#13063,#383);
#348=SHAPE_REPRESENTATION_RELATIONSHIP('SRR','None',#13064,#384);
#349=SHAPE_REPRESENTATION_RELATIONSHIP('SRR','None',#13065,#385);
#350=SHAPE_REPRESENTATION_RELATIONSHIP('SRR','None',#13066,#386);
#351=SHAPE_REPRESENTATION_RELATIONSHIP('SRR','None',#13067,#387);
#352=SHAPE_REPRESENTATION_RELATIONSHIP('SRR','None',#13069,#388);
#353=SHAPE_REPRESENTATION_RELATIONSHIP('SRR','None',#13070,#389);
#354=SHAPE_REPRESENTATION_RELATIONSHIP('SRR','None',#13071,#390);
#355=SHAPE_REPRESENTATION_RELATIONSHIP('SRR','None',#13072,#391);
#356=SHAPE_REPRESENTATION_RELATIONSHIP('SRR','None',#13073,#392);
#357=SHAPE_REPRESENTATION_RELATIONSHIP('SRR','None',#13074,#393);
#358=SHAPE_REPRESENTATION_RELATIONSHIP('SRR','None',#13076,#394);
#359=SHAPE_REPRESENTATION_RELATIONSHIP('SRR','None',#13077,#395);
#360=SHAPE_REPRESENTATION_RELATIONSHIP('SRR','None',#13078,#396);
#361=SHAPE_REPRESENTATION_RELATIONSHIP('SRR','None',#13080,#397);
#362=SHAPE_REPRESENTATION_RELATIONSHIP('SRR','None',#13081,#398);
#363=SHAPE_REPRESENTATION_RELATIONSHIP('SRR','None',#13082,#399);
#364=SHAPE_REPRESENTATION_RELATIONSHIP('SRR','None',#13083,#400);
#365=SHAPE_REPRESENTATION_RELATIONSHIP('SRR','None',#13084,#401);
#366=SHAPE_REPRESENTATION_RELATIONSHIP('SRR','None',#13085,#402);
#367=SHAPE_REPRESENTATION_RELATIONSHIP('SRR','None',#13086,#403);
#368=SHAPE_REPRESENTATION_RELATIONSHIP('SRR','None',#13087,#404);
#369=SHAPE_REPRESENTATION_RELATIONSHIP('SRR','None',#13088,#405);
#370=SHAPE_REPRESENTATION_RELATIONSHIP('SRR','None',#13089,#406);
#371=SHAPE_REPRESENTATION_RELATIONSHIP('SRR','None',#13090,#407);
#372=SHAPE_REPRESENTATION_RELATIONSHIP('SRR','None',#13091,#408);
#373=SHAPE_REPRESENTATION_RELATIONSHIP('SRR','None',#13093,#409);
#374=SHAPE_REPRESENTATION_RELATIONSHIP('SRR','None',#13094,#410);
#375=SHAPE_REPRESENTATION_RELATIONSHIP('SRR','None',#13095,#411);
#376=ADVANCED_BREP_SHAPE_REPRESENTATION('',(#455),#12856);
#377=ADVANCED_BREP_SHAPE_REPRESENTATION('',(#456),#12857);
#378=ADVANCED_BREP_SHAPE_REPRESENTATION('',(#457),#12858);
#379=ADVANCED_BREP_SHAPE_REPRESENTATION('',(#458),#12859);
#380=ADVANCED_BREP_SHAPE_REPRESENTATION('',(#459),#12860);
#381=ADVANCED_BREP_SHAPE_REPRESENTATION('',(#460),#12861);
#382=ADVANCED_BREP_SHAPE_REPRESENTATION('',(#461),#12862);
#383=ADVANCED_BREP_SHAPE_REPRESENTATION('',(#462),#12863);
#384=ADVANCED_BREP_SHAPE_REPRESENTATION('',(#463),#12864);
#385=ADVANCED_BREP_SHAPE_REPRESENTATION('',(#464),#12865);
#386=ADVANCED_BREP_SHAPE_REPRESENTATION('',(#465),#12866);
#387=ADVANCED_BREP_SHAPE_REPRESENTATION('',(#466),#12867);
#388=ADVANCED_BREP_SHAPE_REPRESENTATION('',(#467),#12869);
#389=ADVANCED_BREP_SHAPE_REPRESENTATION('',(#468),#12870);
#390=ADVANCED_BREP_SHAPE_REPRESENTATION('',(#469,#470,#471,#472,#473,#474,
#475),#12871);
#391=ADVANCED_BREP_SHAPE_REPRESENTATION('',(#476),#12872);
#392=ADVANCED_BREP_SHAPE_REPRESENTATION('',(#477,#478),#12873);
#393=ADVANCED_BREP_SHAPE_REPRESENTATION('',(#14),#12874);
#394=ADVANCED_BREP_SHAPE_REPRESENTATION('',(#479),#12876);
#395=ADVANCED_BREP_SHAPE_REPRESENTATION('',(#480),#12877);
#396=ADVANCED_BREP_SHAPE_REPRESENTATION('',(#15),#12878);
#397=ADVANCED_BREP_SHAPE_REPRESENTATION('',(#481),#12880);
#398=ADVANCED_BREP_SHAPE_REPRESENTATION('',(#482),#12881);
#399=ADVANCED_BREP_SHAPE_REPRESENTATION('',(#483),#12882);
#400=ADVANCED_BREP_SHAPE_REPRESENTATION('',(#484),#12883);
#401=ADVANCED_BREP_SHAPE_REPRESENTATION('',(#485),#12884);
#402=ADVANCED_BREP_SHAPE_REPRESENTATION('',(#486),#12885);
#403=ADVANCED_BREP_SHAPE_REPRESENTATION('',(#487),#12886);
#404=ADVANCED_BREP_SHAPE_REPRESENTATION('',(#488),#12887);
#405=ADVANCED_BREP_SHAPE_REPRESENTATION('',(#489),#12888);
#406=ADVANCED_BREP_SHAPE_REPRESENTATION('',(#490),#12889);
#407=ADVANCED_BREP_SHAPE_REPRESENTATION('',(#491),#12890);
#408=ADVANCED_BREP_SHAPE_REPRESENTATION('',(#16),#12891);
#409=ADVANCED_BREP_SHAPE_REPRESENTATION('',(#492),#12893);
#410=ADVANCED_BREP_SHAPE_REPRESENTATION('',(#493),#12894);
#411=ADVANCED_BREP_SHAPE_REPRESENTATION('',(#494),#12895);
#412=STYLED_ITEM('',(#13309),#455);
#413=STYLED_ITEM('',(#13344),#456);
#414=STYLED_ITEM('',(#13344),#457);
#415=STYLED_ITEM('',(#13330),#458);
#416=STYLED_ITEM('',(#13330),#459);
#417=STYLED_ITEM('',(#13330),#460);
#418=STYLED_ITEM('',(#13330),#461);
#419=STYLED_ITEM('',(#13330),#462);
#420=STYLED_ITEM('',(#13330),#463);
#421=STYLED_ITEM('',(#13323),#464);
#422=STYLED_ITEM('',(#13344),#465);
#423=STYLED_ITEM('',(#13330),#466);
#424=STYLED_ITEM('',(#13330),#467);
#425=STYLED_ITEM('',(#13330),#468);
#426=STYLED_ITEM('',(#13330),#469);
#427=STYLED_ITEM('',(#13330),#470);
#428=STYLED_ITEM('',(#13330),#471);
#429=STYLED_ITEM('',(#13330),#472);
#430=STYLED_ITEM('',(#13330),#473);
#431=STYLED_ITEM('',(#13330),#474);
#432=STYLED_ITEM('',(#13330),#475);
#433=STYLED_ITEM('',(#13330),#476);
#434=STYLED_ITEM('',(#13330),#477);
#435=STYLED_ITEM('',(#13330),#478);
#436=STYLED_ITEM('',(#13337),#14);
#437=STYLED_ITEM('',(#13344),#479);
#438=STYLED_ITEM('',(#13323),#480);
#439=STYLED_ITEM('',(#13337),#15);
#440=STYLED_ITEM('',(#13330),#481);
#441=STYLED_ITEM('',(#13330),#482);
#442=STYLED_ITEM('',(#13330),#483);
#443=STYLED_ITEM('',(#13330),#484);
#444=STYLED_ITEM('',(#13330),#485);
#445=STYLED_ITEM('',(#13344),#486);
#446=STYLED_ITEM('',(#13316),#487);
#447=STYLED_ITEM('',(#13337),#488);
#448=STYLED_ITEM('',(#13316),#489);
#449=STYLED_ITEM('',(#13316),#490);
#450=STYLED_ITEM('',(#13330),#491);
#451=STYLED_ITEM('',(#13337),#16);
#452=STYLED_ITEM('',(#13316),#492);
#453=STYLED_ITEM('',(#13344),#493);
#454=STYLED_ITEM('',(#13337),#494);
#455=MANIFOLD_SOLID_BREP('Body1',#6179);
#456=MANIFOLD_SOLID_BREP('Body1',#6180);
#457=MANIFOLD_SOLID_BREP('Body1',#6181);
#458=MANIFOLD_SOLID_BREP('Body1',#6182);
#459=MANIFOLD_SOLID_BREP('Body1',#6183);
#460=MANIFOLD_SOLID_BREP('Body1',#6184);
#461=MANIFOLD_SOLID_BREP('Body1',#6185);
#462=MANIFOLD_SOLID_BREP('Body1',#6186);
#463=MANIFOLD_SOLID_BREP('Body1',#6187);
#464=MANIFOLD_SOLID_BREP('Body1',#6188);
#465=MANIFOLD_SOLID_BREP('Body1',#6189);
#466=MANIFOLD_SOLID_BREP('Body1',#6190);
#467=MANIFOLD_SOLID_BREP('Body1',#6191);
#468=MANIFOLD_SOLID_BREP('Body1',#6192);
#469=MANIFOLD_SOLID_BREP('Body1',#6193);
#470=MANIFOLD_SOLID_BREP('Body2',#6194);
#471=MANIFOLD_SOLID_BREP('Body3',#6195);
#472=MANIFOLD_SOLID_BREP('Body4',#6196);
#473=MANIFOLD_SOLID_BREP('Body5',#6197);
#474=MANIFOLD_SOLID_BREP('Body6',#6198);
#475=MANIFOLD_SOLID_BREP('Body7',#6199);
#476=MANIFOLD_SOLID_BREP('Continuous crown cage',#6200);
#477=MANIFOLD_SOLID_BREP('Body1',#6201);
#478=MANIFOLD_SOLID_BREP('Body2',#6202);
#479=MANIFOLD_SOLID_BREP('Body1',#6205);
#480=MANIFOLD_SOLID_BREP('Body1',#6206);
#481=MANIFOLD_SOLID_BREP('Body1',#6209);
#482=MANIFOLD_SOLID_BREP('Body1',#6210);
#483=MANIFOLD_SOLID_BREP('Body1',#6211);
#484=MANIFOLD_SOLID_BREP('Body1',#6212);
#485=MANIFOLD_SOLID_BREP('Body1',#6213);
#486=MANIFOLD_SOLID_BREP('Body1',#6214);
#487=MANIFOLD_SOLID_BREP('Body1',#6215);
#488=MANIFOLD_SOLID_BREP('Body1',#6216);
#489=MANIFOLD_SOLID_BREP('Body1',#6217);
#490=MANIFOLD_SOLID_BREP('Body1',#6218);
#491=MANIFOLD_SOLID_BREP('Body1',#6219);
#492=MANIFOLD_SOLID_BREP('Body1',#6222);
#493=MANIFOLD_SOLID_BREP('Body1',#6223);
#494=MANIFOLD_SOLID_BREP('Body1',#6224);
#495=FACE_BOUND('',#1479,.T.);
#496=FACE_BOUND('',#1480,.T.);
#497=FACE_BOUND('',#1481,.T.);
#498=FACE_BOUND('',#1482,.T.);
#499=FACE_BOUND('',#1483,.T.);
#500=FACE_BOUND('',#1484,.T.);
#501=FACE_BOUND('',#1485,.T.);
#502=FACE_BOUND('',#1487,.T.);
#503=FACE_BOUND('',#1488,.T.);
#504=FACE_BOUND('',#1489,.T.);
#505=FACE_BOUND('',#1490,.T.);
#506=FACE_BOUND('',#1491,.T.);
#507=FACE_BOUND('',#1492,.T.);
#508=FACE_BOUND('',#1513,.T.);
#509=FACE_BOUND('',#1515,.T.);
#510=FACE_BOUND('',#1519,.T.);
#511=FACE_BOUND('',#1520,.T.);
#512=FACE_BOUND('',#1521,.T.);
#513=FACE_BOUND('',#1522,.T.);
#514=FACE_BOUND('',#1523,.T.);
#515=FACE_BOUND('',#1526,.T.);
#516=FACE_BOUND('',#1527,.T.);
#517=FACE_BOUND('',#1528,.T.);
#518=FACE_BOUND('',#1529,.T.);
#519=FACE_BOUND('',#1530,.T.);
#520=FACE_BOUND('',#1534,.T.);
#521=FACE_BOUND('',#1535,.T.);
#522=FACE_BOUND('',#1542,.T.);
#523=FACE_BOUND('',#1546,.T.);
#524=FACE_BOUND('',#1547,.T.);
#525=FACE_BOUND('',#1548,.T.);
#526=FACE_BOUND('',#1549,.T.);
#527=FACE_BOUND('',#1550,.T.);
#528=FACE_BOUND('',#1552,.T.);
#529=FACE_BOUND('',#1553,.T.);
#530=FACE_BOUND('',#1554,.T.);
#531=FACE_BOUND('',#1555,.T.);
#532=FACE_BOUND('',#1556,.T.);
#533=FACE_BOUND('',#1563,.T.);
#534=FACE_BOUND('',#1567,.T.);
#535=FACE_BOUND('',#1568,.T.);
#536=FACE_BOUND('',#1569,.T.);
#537=FACE_BOUND('',#1570,.T.);
#538=FACE_BOUND('',#1571,.T.);
#539=FACE_BOUND('',#1573,.T.);
#540=FACE_BOUND('',#1574,.T.);
#541=FACE_BOUND('',#1575,.T.);
#542=FACE_BOUND('',#1576,.T.);
#543=FACE_BOUND('',#1577,.T.);
#544=FACE_BOUND('',#1586,.T.);
#545=FACE_BOUND('',#1588,.T.);
#546=FACE_BOUND('',#1592,.T.);
#547=FACE_BOUND('',#1593,.T.);
#548=FACE_BOUND('',#1594,.T.);
#549=FACE_BOUND('',#1595,.T.);
#550=FACE_BOUND('',#1596,.T.);
#551=FACE_BOUND('',#1599,.T.);
#552=FACE_BOUND('',#1600,.T.);
#553=FACE_BOUND('',#1601,.T.);
#554=FACE_BOUND('',#1602,.T.);
#555=FACE_BOUND('',#1603,.T.);
#556=FACE_BOUND('',#1607,.T.);
#557=FACE_BOUND('',#1608,.T.);
#558=FACE_BOUND('',#1615,.T.);
#559=FACE_BOUND('',#1619,.T.);
#560=FACE_BOUND('',#1620,.T.);
#561=FACE_BOUND('',#1621,.T.);
#562=FACE_BOUND('',#1622,.T.);
#563=FACE_BOUND('',#1623,.T.);
#564=FACE_BOUND('',#1625,.T.);
#565=FACE_BOUND('',#1626,.T.);
#566=FACE_BOUND('',#1627,.T.);
#567=FACE_BOUND('',#1628,.T.);
#568=FACE_BOUND('',#1629,.T.);
#569=FACE_BOUND('',#1636,.T.);
#570=FACE_BOUND('',#1640,.T.);
#571=FACE_BOUND('',#1641,.T.);
#572=FACE_BOUND('',#1642,.T.);
#573=FACE_BOUND('',#1643,.T.);
#574=FACE_BOUND('',#1644,.T.);
#575=FACE_BOUND('',#1646,.T.);
#576=FACE_BOUND('',#1647,.T.);
#577=FACE_BOUND('',#1648,.T.);
#578=FACE_BOUND('',#1649,.T.);
#579=FACE_BOUND('',#1650,.T.);
#580=FACE_BOUND('',#1661,.T.);
#581=FACE_BOUND('',#1665,.T.);
#582=FACE_BOUND('',#1669,.T.);
#583=FACE_BOUND('',#1672,.T.);
#584=FACE_BOUND('',#1678,.T.);
#585=FACE_BOUND('',#1686,.T.);
#586=FACE_BOUND('',#1687,.T.);
#587=FACE_BOUND('',#1688,.T.);
#588=FACE_BOUND('',#1689,.T.);
#589=FACE_BOUND('',#1690,.T.);
#590=FACE_BOUND('',#1691,.T.);
#591=FACE_BOUND('',#1692,.T.);
#592=FACE_BOUND('',#1694,.T.);
#593=FACE_BOUND('',#1701,.T.);
#594=FACE_BOUND('',#1705,.T.);
#595=FACE_BOUND('',#1706,.T.);
#596=FACE_BOUND('',#1707,.T.);
#597=FACE_BOUND('',#1708,.T.);
#598=FACE_BOUND('',#1709,.T.);
#599=FACE_BOUND('',#1711,.T.);
#600=FACE_BOUND('',#1712,.T.);
#601=FACE_BOUND('',#1713,.T.);
#602=FACE_BOUND('',#1714,.T.);
#603=FACE_BOUND('',#1715,.T.);
#604=FACE_BOUND('',#1724,.T.);
#605=FACE_BOUND('',#1727,.T.);
#606=FACE_BOUND('',#1732,.T.);
#607=FACE_BOUND('',#1737,.T.);
#608=FACE_BOUND('',#1762,.T.);
#609=FACE_BOUND('',#1765,.T.);
#610=FACE_BOUND('',#1768,.T.);
#611=FACE_BOUND('',#1771,.T.);
#612=FACE_BOUND('',#1774,.T.);
#613=FACE_BOUND('',#1781,.T.);
#614=FACE_BOUND('',#1800,.T.);
#615=FACE_BOUND('',#1803,.T.);
#616=FACE_BOUND('',#1806,.T.);
#617=FACE_BOUND('',#1809,.T.);
#618=FACE_BOUND('',#1812,.T.);
#619=FACE_BOUND('',#1815,.T.);
#620=FACE_BOUND('',#1817,.T.);
#621=FACE_BOUND('',#1823,.T.);
#622=FACE_BOUND('',#1825,.T.);
#623=FACE_BOUND('',#1827,.T.);
#624=FACE_BOUND('',#1829,.T.);
#625=FACE_BOUND('',#1844,.T.);
#626=FACE_BOUND('',#1862,.T.);
#627=FACE_BOUND('',#1863,.T.);
#628=FACE_BOUND('',#1865,.T.);
#629=FACE_BOUND('',#1867,.T.);
#630=FACE_BOUND('',#1871,.T.);
#631=FACE_BOUND('',#1873,.T.);
#632=FACE_BOUND('',#1877,.T.);
#633=FACE_BOUND('',#1879,.T.);
#634=FACE_BOUND('',#1883,.T.);
#635=FACE_BOUND('',#1885,.T.);
#636=FACE_BOUND('',#1889,.T.);
#637=FACE_BOUND('',#1891,.T.);
#638=FACE_BOUND('',#1896,.T.);
#639=FACE_BOUND('',#1901,.T.);
#640=FACE_BOUND('',#1904,.T.);
#641=FACE_BOUND('',#1906,.T.);
#642=FACE_BOUND('',#1912,.T.);
#643=FACE_BOUND('',#1916,.T.);
#644=FACE_BOUND('',#1920,.T.);
#645=FACE_BOUND('',#1922,.T.);
#646=FACE_BOUND('',#1924,.T.);
#647=FACE_BOUND('',#1930,.T.);
#648=FACE_BOUND('',#1934,.T.);
#649=FACE_BOUND('',#1936,.T.);
#650=FACE_BOUND('',#1940,.T.);
#651=FACE_BOUND('',#1942,.T.);
#652=FACE_BOUND('',#1958,.T.);
#653=FACE_BOUND('',#1977,.T.);
#654=FACE_BOUND('',#1979,.T.);
#655=FACE_BOUND('',#1981,.T.);
#656=FACE_BOUND('',#1988,.T.);
#657=FACE_BOUND('',#1992,.T.);
#658=FACE_BOUND('',#1994,.T.);
#659=CIRCLE('',#6631,0.21);
#660=CIRCLE('',#6632,0.21);
#661=CIRCLE('',#6634,0.21);
#662=CIRCLE('',#6635,0.21);
#663=CIRCLE('',#6637,0.165);
#664=CIRCLE('',#6638,0.165);
#665=CIRCLE('',#6640,0.165);
#666=CIRCLE('',#6641,0.165);
#667=CIRCLE('',#6643,0.165);
#668=CIRCLE('',#6644,0.165);
#669=CIRCLE('',#6646,0.165);
#670=CIRCLE('',#6647,0.165);
#671=CIRCLE('',#6670,0.225);
#672=CIRCLE('',#6671,0.225);
#673=CIRCLE('',#6673,0.225);
#674=CIRCLE('',#6674,0.225);
#675=CIRCLE('',#6676,0.165);
#676=CIRCLE('',#6677,0.165);
#677=CIRCLE('',#6679,0.165);
#678=CIRCLE('',#6680,0.165);
#679=CIRCLE('',#6682,0.165);
#680=CIRCLE('',#6683,0.165);
#681=CIRCLE('',#6685,0.165);
#682=CIRCLE('',#6686,0.165);
#683=CIRCLE('',#6688,1.6);
#684=CIRCLE('',#6689,1.6);
#685=CIRCLE('',#6702,0.225);
#686=CIRCLE('',#6703,0.225);
#687=CIRCLE('',#6705,0.225);
#688=CIRCLE('',#6706,0.225);
#689=CIRCLE('',#6708,0.225);
#690=CIRCLE('',#6709,0.225);
#691=CIRCLE('',#6711,0.225);
#692=CIRCLE('',#6712,0.225);
#693=CIRCLE('',#6714,1.59);
#694=CIRCLE('',#6715,1.59);
#695=CIRCLE('',#6717,1.005);
#696=CIRCLE('',#6719,1.005);
#697=CIRCLE('',#6721,2.4);
#698=CIRCLE('',#6722,2.4);
#699=CIRCLE('',#6727,0.225);
#700=CIRCLE('',#6728,0.225);
#701=CIRCLE('',#6730,0.225);
#702=CIRCLE('',#6731,0.225);
#703=CIRCLE('',#6733,0.225);
#704=CIRCLE('',#6734,0.225);
#705=CIRCLE('',#6736,0.225);
#706=CIRCLE('',#6737,0.225);
#707=CIRCLE('',#6739,1.59);
#708=CIRCLE('',#6740,1.59);
#709=CIRCLE('',#6742,1.005);
#710=CIRCLE('',#6744,1.005);
#711=CIRCLE('',#6746,2.4);
#712=CIRCLE('',#6747,2.4);
#713=CIRCLE('',#6752,0.225);
#714=CIRCLE('',#6753,0.225);
#715=CIRCLE('',#6755,0.225);
#716=CIRCLE('',#6756,0.225);
#717=CIRCLE('',#6758,0.165);
#718=CIRCLE('',#6759,0.165);
#719=CIRCLE('',#6761,0.165);
#720=CIRCLE('',#6762,0.165);
#721=CIRCLE('',#6764,0.165);
#722=CIRCLE('',#6765,0.165);
#723=CIRCLE('',#6767,0.165);
#724=CIRCLE('',#6768,0.165);
#725=CIRCLE('',#6770,1.6);
#726=CIRCLE('',#6771,1.6);
#727=CIRCLE('',#6784,0.225);
#728=CIRCLE('',#6785,0.225);
#729=CIRCLE('',#6787,0.225);
#730=CIRCLE('',#6788,0.225);
#731=CIRCLE('',#6790,0.225);
#732=CIRCLE('',#6791,0.225);
#733=CIRCLE('',#6793,0.225);
#734=CIRCLE('',#6794,0.225);
#735=CIRCLE('',#6796,1.59);
#736=CIRCLE('',#6797,1.59);
#737=CIRCLE('',#6799,1.005);
#738=CIRCLE('',#6801,1.005);
#739=CIRCLE('',#6803,2.4);
#740=CIRCLE('',#6804,2.4);
#741=CIRCLE('',#6809,0.225);
#742=CIRCLE('',#6810,0.225);
#743=CIRCLE('',#6812,0.225);
#744=CIRCLE('',#6813,0.225);
#745=CIRCLE('',#6815,0.225);
#746=CIRCLE('',#6816,0.225);
#747=CIRCLE('',#6818,0.225);
#748=CIRCLE('',#6819,0.225);
#749=CIRCLE('',#6821,1.59);
#750=CIRCLE('',#6822,1.59);
#751=CIRCLE('',#6824,1.005);
#752=CIRCLE('',#6826,1.005);
#753=CIRCLE('',#6828,2.4);
#754=CIRCLE('',#6829,2.4);
#755=CIRCLE('',#6834,0.165);
#756=CIRCLE('',#6835,0.165);
#757=CIRCLE('',#6838,0.165);
#758=CIRCLE('',#6839,0.165);
#759=CIRCLE('',#6842,0.165);
#760=CIRCLE('',#6843,0.165);
#761=CIRCLE('',#6846,0.165);
#762=CIRCLE('',#6847,0.165);
#763=CIRCLE('',#6850,1.05);
#764=CIRCLE('',#6851,1.05);
#765=CIRCLE('',#6853,0.625);
#766=CIRCLE('',#6855,0.625);
#767=CIRCLE('',#6857,0.5);
#768=CIRCLE('',#6858,0.5);
#769=CIRCLE('',#6860,0.275);
#770=CIRCLE('',#6862,0.275);
#771=CIRCLE('',#6864,0.5);
#772=CIRCLE('',#6865,0.5);
#773=CIRCLE('',#6867,0.275);
#774=CIRCLE('',#6869,0.275);
#775=CIRCLE('',#6886,0.225);
#776=CIRCLE('',#6887,0.225);
#777=CIRCLE('',#6889,0.225);
#778=CIRCLE('',#6890,0.225);
#779=CIRCLE('',#6892,0.225);
#780=CIRCLE('',#6893,0.225);
#781=CIRCLE('',#6895,0.225);
#782=CIRCLE('',#6896,0.225);
#783=CIRCLE('',#6898,1.04);
#784=CIRCLE('',#6899,1.04);
#785=CIRCLE('',#6901,0.625);
#786=CIRCLE('',#6903,0.625);
#787=CIRCLE('',#6905,1.8);
#788=CIRCLE('',#6906,1.8);
#789=CIRCLE('',#6910,0.075);
#790=CIRCLE('',#6911,0.075);
#791=CIRCLE('',#6917,1.070235);
#792=CIRCLE('',#6918,1.070235);
#793=CIRCLE('',#6919,0.309556);
#794=CIRCLE('',#6920,1.070235);
#795=CIRCLE('',#6921,1.070235);
#796=CIRCLE('',#6923,1.070235);
#797=CIRCLE('',#6925,0.6);
#798=CIRCLE('',#6926,0.6);
#799=CIRCLE('',#6928,0.66);
#800=CIRCLE('',#6931,1.070235);
#801=CIRCLE('',#6933,0.66);
#802=CIRCLE('',#6937,1.129765);
#803=CIRCLE('',#6938,1.129765);
#804=CIRCLE('',#6939,0.309556);
#805=CIRCLE('',#6940,1.129765);
#806=CIRCLE('',#6941,1.129765);
#807=CIRCLE('',#6943,1.129765);
#808=CIRCLE('',#6945,1.54);
#809=CIRCLE('',#6946,1.129765);
#810=CIRCLE('',#6948,1.6);
#811=CIRCLE('',#6950,1.6);
#812=CIRCLE('',#6952,1.54);
#813=CIRCLE('',#6957,0.29765);
#814=CIRCLE('',#6959,0.29765);
#815=CIRCLE('',#6961,0.29765);
#816=CIRCLE('',#6963,0.29765);
#817=CIRCLE('',#6965,0.29765);
#818=CIRCLE('',#6967,0.29765);
#819=CIRCLE('',#6969,0.29765);
#820=CIRCLE('',#6972,0.303778037777585);
#821=CIRCLE('',#6973,0.303778037777585);
#822=CIRCLE('',#6975,1.123812);
#823=CIRCLE('',#6976,1.123812);
#824=CIRCLE('',#6977,1.123812);
#825=CIRCLE('',#6978,1.123812);
#826=CIRCLE('',#6979,1.123812);
#827=CIRCLE('',#6980,1.123812);
#828=CIRCLE('',#6981,1.123812);
#829=CIRCLE('',#6982,1.123812);
#830=CIRCLE('',#6983,1.123812);
#831=CIRCLE('',#6985,1.076188);
#832=CIRCLE('',#6986,0.303778037777585);
#833=CIRCLE('',#6988,0.303778037777585);
#834=CIRCLE('',#6990,1.076188);
#835=CIRCLE('',#6991,0.303778037777585);
#836=CIRCLE('',#6993,0.303778037777585);
#837=CIRCLE('',#6995,1.076188);
#838=CIRCLE('',#6996,1.076188);
#839=CIRCLE('',#6997,0.303778037777585);
#840=CIRCLE('',#6999,0.303778037777585);
#841=CIRCLE('',#7001,1.076188);
#842=CIRCLE('',#7002,0.303778037777585);
#843=CIRCLE('',#7004,0.303778037777585);
#844=CIRCLE('',#7006,1.076188);
#845=CIRCLE('',#7007,0.303778037777585);
#846=CIRCLE('',#7009,0.303778037777585);
#847=CIRCLE('',#7011,1.076188);
#848=CIRCLE('',#7012,1.076188);
#849=CIRCLE('',#7013,1.076188);
#850=CIRCLE('',#7015,0.303778037777585);
#851=CIRCLE('',#7017,0.303778037777585);
#852=CIRCLE('',#7022,1.119765);
#853=CIRCLE('',#7023,1.085235);
#854=CIRCLE('',#7025,1.119765);
#855=CIRCLE('',#7027,1.085235);
#856=CIRCLE('',#7030,1.119765);
#857=CIRCLE('',#7031,1.085235);
#858=CIRCLE('',#7033,1.119765);
#859=CIRCLE('',#7035,1.085235);
#860=CIRCLE('',#7044,0.375);
#861=CIRCLE('',#7046,0.425);
#862=CIRCLE('',#7048,0.425);
#863=CIRCLE('',#7050,0.395);
#864=CIRCLE('',#7052,0.27);
#865=CIRCLE('',#7054,0.24505);
#866=CIRCLE('',#7056,0.24505);
#867=CIRCLE('',#7058,0.2);
#868=CIRCLE('',#7071,0.9);
#869=CIRCLE('',#7074,0.9);
#870=CIRCLE('',#7078,1.05);
#871=CIRCLE('',#7079,0.9);
#872=CIRCLE('',#7081,1.05);
#873=CIRCLE('',#7083,1.);
#874=CIRCLE('',#7085,1.);
#875=CIRCLE('',#7087,1.05);
#876=CIRCLE('',#7089,1.05);
#877=CIRCLE('',#7091,1.);
#878=CIRCLE('',#7093,1.);
#879=CIRCLE('',#7095,1.05);
#880=CIRCLE('',#7097,1.05);
#881=CIRCLE('',#7099,0.9);
#882=CIRCLE('',#7103,0.895);
#883=CIRCLE('',#7104,0.605);
#884=CIRCLE('',#7107,0.895);
#885=CIRCLE('',#7108,0.605);
#886=CIRCLE('',#7111,0.895);
#887=CIRCLE('',#7112,0.605);
#888=CIRCLE('',#7114,0.895);
#889=CIRCLE('',#7116,0.605);
#890=CIRCLE('',#7130,0.1954);
#891=CIRCLE('',#7132,0.3);
#892=CIRCLE('',#7134,0.35);
#893=CIRCLE('',#7136,0.35);
#894=CIRCLE('',#7138,0.32);
#895=CIRCLE('',#7140,0.22);
#896=CIRCLE('',#7142,0.1954);
#897=CIRCLE('',#7147,0.165);
#898=CIRCLE('',#7148,0.165);
#899=CIRCLE('',#7151,0.165);
#900=CIRCLE('',#7152,0.165);
#901=CIRCLE('',#7156,0.6);
#902=CIRCLE('',#7160,0.6);
#903=CIRCLE('',#7163,0.6);
#904=CIRCLE('',#7167,0.6);
#905=CIRCLE('',#7169,0.6);
#906=CIRCLE('',#7170,0.6);
#907=CIRCLE('',#7175,0.605);
#908=CIRCLE('',#7176,0.605);
#909=CIRCLE('',#7178,0.8);
#910=CIRCLE('',#7179,0.8);
#911=CIRCLE('',#7184,0.605);
#912=CIRCLE('',#7185,0.605);
#913=CIRCLE('',#7187,0.8);
#914=CIRCLE('',#7188,0.8);
#915=CIRCLE('',#7193,0.605);
#916=CIRCLE('',#7194,0.605);
#917=CIRCLE('',#7196,0.8);
#918=CIRCLE('',#7197,0.8);
#919=CIRCLE('',#7202,0.605);
#920=CIRCLE('',#7203,0.605);
#921=CIRCLE('',#7205,0.8);
#922=CIRCLE('',#7206,0.8);
#923=CIRCLE('',#7214,1.2);
#924=CIRCLE('',#7215,0.6);
#925=CIRCLE('',#7217,0.6);
#926=CIRCLE('',#7219,1.2);
#927=CIRCLE('',#7220,1.2);
#928=CIRCLE('',#7222,1.2);
#929=CIRCLE('',#7225,2.);
#930=CIRCLE('',#7226,2.);
#931=CIRCLE('',#7231,0.225);
#932=CIRCLE('',#7232,0.225);
#933=CIRCLE('',#7237,1.2);
#934=CIRCLE('',#7238,0.6);
#935=CIRCLE('',#7240,0.6);
#936=CIRCLE('',#7242,0.7);
#937=CIRCLE('',#7243,0.7);
#938=CIRCLE('',#7245,1.2);
#939=CIRCLE('',#7249,1.2);
#940=CIRCLE('',#7251,1.2);
#941=CIRCLE('',#7255,0.165);
#942=CIRCLE('',#7256,0.165);
#943=CIRCLE('',#7259,0.6);
#944=CIRCLE('',#7260,0.6);
#945=CIRCLE('',#7265,0.225);
#946=CIRCLE('',#7266,0.225);
#947=CIRCLE('',#7268,1.);
#948=CIRCLE('',#7269,1.);
#949=CIRCLE('',#7274,0.225);
#950=CIRCLE('',#7275,0.225);
#951=CIRCLE('',#7277,1.);
#952=CIRCLE('',#7278,1.);
#953=CIRCLE('',#7294,0.3);
#954=CIRCLE('',#7296,0.35);
#955=CIRCLE('',#7298,0.35);
#956=CIRCLE('',#7300,0.32);
#957=CIRCLE('',#7302,0.22);
#958=CIRCLE('',#7304,0.1954);
#959=CIRCLE('',#7306,0.1954);
#960=CIRCLE('',#7308,0.16);
#961=CIRCLE('',#7377,0.425);
#962=CIRCLE('',#7378,0.425);
#963=CIRCLE('',#7387,0.9);
#964=CIRCLE('',#7388,0.6);
#965=CIRCLE('',#7390,0.9);
#966=CIRCLE('',#7393,0.5);
#967=CIRCLE('',#7394,0.5);
#968=CIRCLE('',#7397,0.6);
#969=CIRCLE('',#7401,0.605);
#970=CIRCLE('',#7402,0.605);
#971=CIRCLE('',#7404,1.25);
#972=CIRCLE('',#7405,1.25);
#973=CYLINDRICAL_SURFACE('',#6630,0.21);
#974=CYLINDRICAL_SURFACE('',#6633,0.21);
#975=CYLINDRICAL_SURFACE('',#6636,0.165);
#976=CYLINDRICAL_SURFACE('',#6639,0.165);
#977=CYLINDRICAL_SURFACE('',#6642,0.165);
#978=CYLINDRICAL_SURFACE('',#6645,0.165);
#979=CYLINDRICAL_SURFACE('',#6669,0.225);
#980=CYLINDRICAL_SURFACE('',#6672,0.225);
#981=CYLINDRICAL_SURFACE('',#6675,0.165);
#982=CYLINDRICAL_SURFACE('',#6678,0.165);
#983=CYLINDRICAL_SURFACE('',#6681,0.165);
#984=CYLINDRICAL_SURFACE('',#6684,0.165);
#985=CYLINDRICAL_SURFACE('',#6687,1.6);
#986=CYLINDRICAL_SURFACE('',#6701,0.225);
#987=CYLINDRICAL_SURFACE('',#6704,0.225);
#988=CYLINDRICAL_SURFACE('',#6707,0.225);
#989=CYLINDRICAL_SURFACE('',#6710,0.225);
#990=CYLINDRICAL_SURFACE('',#6713,1.59);
#991=CYLINDRICAL_SURFACE('',#6718,1.005);
#992=CYLINDRICAL_SURFACE('',#6720,2.4);
#993=CYLINDRICAL_SURFACE('',#6726,0.225);
#994=CYLINDRICAL_SURFACE('',#6729,0.225);
#995=CYLINDRICAL_SURFACE('',#6732,0.225);
#996=CYLINDRICAL_SURFACE('',#6735,0.225);
#997=CYLINDRICAL_SURFACE('',#6738,1.59);
#998=CYLINDRICAL_SURFACE('',#6743,1.005);
#999=CYLINDRICAL_SURFACE('',#6745,2.4);
#1000=CYLINDRICAL_SURFACE('',#6751,0.225);
#1001=CYLINDRICAL_SURFACE('',#6754,0.225);
#1002=CYLINDRICAL_SURFACE('',#6757,0.165);
#1003=CYLINDRICAL_SURFACE('',#6760,0.165);
#1004=CYLINDRICAL_SURFACE('',#6763,0.165);
#1005=CYLINDRICAL_SURFACE('',#6766,0.165);
#1006=CYLINDRICAL_SURFACE('',#6769,1.6);
#1007=CYLINDRICAL_SURFACE('',#6783,0.225);
#1008=CYLINDRICAL_SURFACE('',#6786,0.225);
#1009=CYLINDRICAL_SURFACE('',#6789,0.225);
#1010=CYLINDRICAL_SURFACE('',#6792,0.225);
#1011=CYLINDRICAL_SURFACE('',#6795,1.59);
#1012=CYLINDRICAL_SURFACE('',#6800,1.005);
#1013=CYLINDRICAL_SURFACE('',#6802,2.4);
#1014=CYLINDRICAL_SURFACE('',#6808,0.225);
#1015=CYLINDRICAL_SURFACE('',#6811,0.225);
#1016=CYLINDRICAL_SURFACE('',#6814,0.225);
#1017=CYLINDRICAL_SURFACE('',#6817,0.225);
#1018=CYLINDRICAL_SURFACE('',#6820,1.59);
#1019=CYLINDRICAL_SURFACE('',#6825,1.005);
#1020=CYLINDRICAL_SURFACE('',#6827,2.4);
#1021=CYLINDRICAL_SURFACE('',#6833,0.165);
#1022=CYLINDRICAL_SURFACE('',#6837,0.165);
#1023=CYLINDRICAL_SURFACE('',#6841,0.165);
#1024=CYLINDRICAL_SURFACE('',#6845,0.165);
#1025=CYLINDRICAL_SURFACE('',#6849,1.05);
#1026=CYLINDRICAL_SURFACE('',#6854,0.625);
#1027=CYLINDRICAL_SURFACE('',#6856,0.5);
#1028=CYLINDRICAL_SURFACE('',#6861,0.275);
#1029=CYLINDRICAL_SURFACE('',#6863,0.5);
#1030=CYLINDRICAL_SURFACE('',#6868,0.275);
#1031=CYLINDRICAL_SURFACE('',#6885,0.225);
#1032=CYLINDRICAL_SURFACE('',#6888,0.225);
#1033=CYLINDRICAL_SURFACE('',#6891,0.225);
#1034=CYLINDRICAL_SURFACE('',#6894,0.225);
#1035=CYLINDRICAL_SURFACE('',#6897,1.04);
#1036=CYLINDRICAL_SURFACE('',#6902,0.625);
#1037=CYLINDRICAL_SURFACE('',#6904,1.8);
#1038=CYLINDRICAL_SURFACE('',#6922,1.070235);
#1039=CYLINDRICAL_SURFACE('',#6924,0.6);
#1040=CYLINDRICAL_SURFACE('',#6930,1.070235);
#1041=CYLINDRICAL_SURFACE('',#6942,1.129765);
#1042=CYLINDRICAL_SURFACE('',#6949,1.6);
#1043=CYLINDRICAL_SURFACE('',#6954,1.129765);
#1044=CYLINDRICAL_SURFACE('',#6974,1.123812);
#1045=CYLINDRICAL_SURFACE('',#7010,1.076188);
#1046=CYLINDRICAL_SURFACE('',#7024,1.119765);
#1047=CYLINDRICAL_SURFACE('',#7028,1.085235);
#1048=CYLINDRICAL_SURFACE('',#7032,1.119765);
#1049=CYLINDRICAL_SURFACE('',#7036,1.085235);
#1050=CYLINDRICAL_SURFACE('',#7047,0.425);
#1051=CYLINDRICAL_SURFACE('',#7055,0.24505);
#1052=CYLINDRICAL_SURFACE('',#7080,1.05);
#1053=CYLINDRICAL_SURFACE('',#7084,1.);
#1054=CYLINDRICAL_SURFACE('',#7088,1.05);
#1055=CYLINDRICAL_SURFACE('',#7092,1.);
#1056=CYLINDRICAL_SURFACE('',#7096,1.05);
#1057=CYLINDRICAL_SURFACE('',#7100,0.9);
#1058=CYLINDRICAL_SURFACE('',#7113,0.895);
#1059=CYLINDRICAL_SURFACE('',#7117,0.605);
#1060=CYLINDRICAL_SURFACE('',#7135,0.35);
#1061=CYLINDRICAL_SURFACE('',#7143,0.1954);
#1062=CYLINDRICAL_SURFACE('',#7146,0.165);
#1063=CYLINDRICAL_SURFACE('',#7150,0.165);
#1064=CYLINDRICAL_SURFACE('',#7168,0.6);
#1065=CYLINDRICAL_SURFACE('',#7174,0.605);
#1066=CYLINDRICAL_SURFACE('',#7177,0.8);
#1067=CYLINDRICAL_SURFACE('',#7183,0.605);
#1068=CYLINDRICAL_SURFACE('',#7186,0.8);
#1069=CYLINDRICAL_SURFACE('',#7192,0.605);
#1070=CYLINDRICAL_SURFACE('',#7195,0.8);
#1071=CYLINDRICAL_SURFACE('',#7201,0.605);
#1072=CYLINDRICAL_SURFACE('',#7204,0.8);
#1073=CYLINDRICAL_SURFACE('',#7216,0.6);
#1074=CYLINDRICAL_SURFACE('',#7218,1.2);
#1075=CYLINDRICAL_SURFACE('',#7221,1.2);
#1076=CYLINDRICAL_SURFACE('',#7224,2.);
#1077=CYLINDRICAL_SURFACE('',#7230,0.225);
#1078=CYLINDRICAL_SURFACE('',#7239,0.6);
#1079=CYLINDRICAL_SURFACE('',#7241,0.7);
#1080=CYLINDRICAL_SURFACE('',#7250,1.2);
#1081=CYLINDRICAL_SURFACE('',#7254,0.165);
#1082=CYLINDRICAL_SURFACE('',#7258,0.6);
#1083=CYLINDRICAL_SURFACE('',#7264,0.225);
#1084=CYLINDRICAL_SURFACE('',#7267,1.);
#1085=CYLINDRICAL_SURFACE('',#7273,0.225);
#1086=CYLINDRICAL_SURFACE('',#7276,1.);
#1087=CYLINDRICAL_SURFACE('',#7297,0.35);
#1088=CYLINDRICAL_SURFACE('',#7305,0.1954);
#1089=CYLINDRICAL_SURFACE('',#7376,0.425);
#1090=CYLINDRICAL_SURFACE('',#7389,0.9);
#1091=CYLINDRICAL_SURFACE('',#7392,0.5);
#1092=CYLINDRICAL_SURFACE('',#7396,0.6);
#1093=CYLINDRICAL_SURFACE('',#7400,0.605);
#1094=CYLINDRICAL_SURFACE('',#7403,1.25);
#1095=FACE_OUTER_BOUND('',#1463,.T.);
#1096=FACE_OUTER_BOUND('',#1464,.T.);
#1097=FACE_OUTER_BOUND('',#1465,.T.);
#1098=FACE_OUTER_BOUND('',#1466,.T.);
#1099=FACE_OUTER_BOUND('',#1467,.T.);
#1100=FACE_OUTER_BOUND('',#1468,.T.);
#1101=FACE_OUTER_BOUND('',#1469,.T.);
#1102=FACE_OUTER_BOUND('',#1470,.T.);
#1103=FACE_OUTER_BOUND('',#1471,.T.);
#1104=FACE_OUTER_BOUND('',#1472,.T.);
#1105=FACE_OUTER_BOUND('',#1473,.T.);
#1106=FACE_OUTER_BOUND('',#1474,.T.);
#1107=FACE_OUTER_BOUND('',#1475,.T.);
#1108=FACE_OUTER_BOUND('',#1476,.T.);
#1109=FACE_OUTER_BOUND('',#1477,.T.);
#1110=FACE_OUTER_BOUND('',#1478,.T.);
#1111=FACE_OUTER_BOUND('',#1486,.T.);
#1112=FACE_OUTER_BOUND('',#1493,.T.);
#1113=FACE_OUTER_BOUND('',#1494,.T.);
#1114=FACE_OUTER_BOUND('',#1495,.T.);
#1115=FACE_OUTER_BOUND('',#1496,.T.);
#1116=FACE_OUTER_BOUND('',#1497,.T.);
#1117=FACE_OUTER_BOUND('',#1498,.T.);
#1118=FACE_OUTER_BOUND('',#1499,.T.);
#1119=FACE_OUTER_BOUND('',#1500,.T.);
#1120=FACE_OUTER_BOUND('',#1501,.T.);
#1121=FACE_OUTER_BOUND('',#1502,.T.);
#1122=FACE_OUTER_BOUND('',#1503,.T.);
#1123=FACE_OUTER_BOUND('',#1504,.T.);
#1124=FACE_OUTER_BOUND('',#1505,.T.);
#1125=FACE_OUTER_BOUND('',#1506,.T.);
#1126=FACE_OUTER_BOUND('',#1507,.T.);
#1127=FACE_OUTER_BOUND('',#1508,.T.);
#1128=FACE_OUTER_BOUND('',#1509,.T.);
#1129=FACE_OUTER_BOUND('',#1510,.T.);
#1130=FACE_OUTER_BOUND('',#1511,.T.);
#1131=FACE_OUTER_BOUND('',#1512,.T.);
#1132=FACE_OUTER_BOUND('',#1514,.T.);
#1133=FACE_OUTER_BOUND('',#1516,.T.);
#1134=FACE_OUTER_BOUND('',#1517,.T.);
#1135=FACE_OUTER_BOUND('',#1518,.T.);
#1136=FACE_OUTER_BOUND('',#1524,.T.);
#1137=FACE_OUTER_BOUND('',#1525,.T.);
#1138=FACE_OUTER_BOUND('',#1531,.T.);
#1139=FACE_OUTER_BOUND('',#1532,.T.);
#1140=FACE_OUTER_BOUND('',#1533,.T.);
#1141=FACE_OUTER_BOUND('',#1536,.T.);
#1142=FACE_OUTER_BOUND('',#1537,.T.);
#1143=FACE_OUTER_BOUND('',#1538,.T.);
#1144=FACE_OUTER_BOUND('',#1539,.T.);
#1145=FACE_OUTER_BOUND('',#1540,.T.);
#1146=FACE_OUTER_BOUND('',#1541,.T.);
#1147=FACE_OUTER_BOUND('',#1543,.T.);
#1148=FACE_OUTER_BOUND('',#1544,.T.);
#1149=FACE_OUTER_BOUND('',#1545,.T.);
#1150=FACE_OUTER_BOUND('',#1551,.T.);
#1151=FACE_OUTER_BOUND('',#1557,.T.);
#1152=FACE_OUTER_BOUND('',#1558,.T.);
#1153=FACE_OUTER_BOUND('',#1559,.T.);
#1154=FACE_OUTER_BOUND('',#1560,.T.);
#1155=FACE_OUTER_BOUND('',#1561,.T.);
#1156=FACE_OUTER_BOUND('',#1562,.T.);
#1157=FACE_OUTER_BOUND('',#1564,.T.);
#1158=FACE_OUTER_BOUND('',#1565,.T.);
#1159=FACE_OUTER_BOUND('',#1566,.T.);
#1160=FACE_OUTER_BOUND('',#1572,.T.);
#1161=FACE_OUTER_BOUND('',#1578,.T.);
#1162=FACE_OUTER_BOUND('',#1579,.T.);
#1163=FACE_OUTER_BOUND('',#1580,.T.);
#1164=FACE_OUTER_BOUND('',#1581,.T.);
#1165=FACE_OUTER_BOUND('',#1582,.T.);
#1166=FACE_OUTER_BOUND('',#1583,.T.);
#1167=FACE_OUTER_BOUND('',#1584,.T.);
#1168=FACE_OUTER_BOUND('',#1585,.T.);
#1169=FACE_OUTER_BOUND('',#1587,.T.);
#1170=FACE_OUTER_BOUND('',#1589,.T.);
#1171=FACE_OUTER_BOUND('',#1590,.T.);
#1172=FACE_OUTER_BOUND('',#1591,.T.);
#1173=FACE_OUTER_BOUND('',#1597,.T.);
#1174=FACE_OUTER_BOUND('',#1598,.T.);
#1175=FACE_OUTER_BOUND('',#1604,.T.);
#1176=FACE_OUTER_BOUND('',#1605,.T.);
#1177=FACE_OUTER_BOUND('',#1606,.T.);
#1178=FACE_OUTER_BOUND('',#1609,.T.);
#1179=FACE_OUTER_BOUND('',#1610,.T.);
#1180=FACE_OUTER_BOUND('',#1611,.T.);
#1181=FACE_OUTER_BOUND('',#1612,.T.);
#1182=FACE_OUTER_BOUND('',#1613,.T.);
#1183=FACE_OUTER_BOUND('',#1614,.T.);
#1184=FACE_OUTER_BOUND('',#1616,.T.);
#1185=FACE_OUTER_BOUND('',#1617,.T.);
#1186=FACE_OUTER_BOUND('',#1618,.T.);
#1187=FACE_OUTER_BOUND('',#1624,.T.);
#1188=FACE_OUTER_BOUND('',#1630,.T.);
#1189=FACE_OUTER_BOUND('',#1631,.T.);
#1190=FACE_OUTER_BOUND('',#1632,.T.);
#1191=FACE_OUTER_BOUND('',#1633,.T.);
#1192=FACE_OUTER_BOUND('',#1634,.T.);
#1193=FACE_OUTER_BOUND('',#1635,.T.);
#1194=FACE_OUTER_BOUND('',#1637,.T.);
#1195=FACE_OUTER_BOUND('',#1638,.T.);
#1196=FACE_OUTER_BOUND('',#1639,.T.);
#1197=FACE_OUTER_BOUND('',#1645,.T.);
#1198=FACE_OUTER_BOUND('',#1651,.T.);
#1199=FACE_OUTER_BOUND('',#1652,.T.);
#1200=FACE_OUTER_BOUND('',#1653,.T.);
#1201=FACE_OUTER_BOUND('',#1654,.T.);
#1202=FACE_OUTER_BOUND('',#1655,.T.);
#1203=FACE_OUTER_BOUND('',#1656,.T.);
#1204=FACE_OUTER_BOUND('',#1657,.T.);
#1205=FACE_OUTER_BOUND('',#1658,.T.);
#1206=FACE_OUTER_BOUND('',#1659,.T.);
#1207=FACE_OUTER_BOUND('',#1660,.T.);
#1208=FACE_OUTER_BOUND('',#1662,.T.);
#1209=FACE_OUTER_BOUND('',#1663,.T.);
#1210=FACE_OUTER_BOUND('',#1664,.T.);
#1211=FACE_OUTER_BOUND('',#1666,.T.);
#1212=FACE_OUTER_BOUND('',#1667,.T.);
#1213=FACE_OUTER_BOUND('',#1668,.T.);
#1214=FACE_OUTER_BOUND('',#1670,.T.);
#1215=FACE_OUTER_BOUND('',#1671,.T.);
#1216=FACE_OUTER_BOUND('',#1673,.T.);
#1217=FACE_OUTER_BOUND('',#1674,.T.);
#1218=FACE_OUTER_BOUND('',#1675,.T.);
#1219=FACE_OUTER_BOUND('',#1676,.T.);
#1220=FACE_OUTER_BOUND('',#1677,.T.);
#1221=FACE_OUTER_BOUND('',#1679,.T.);
#1222=FACE_OUTER_BOUND('',#1680,.T.);
#1223=FACE_OUTER_BOUND('',#1681,.T.);
#1224=FACE_OUTER_BOUND('',#1682,.T.);
#1225=FACE_OUTER_BOUND('',#1683,.T.);
#1226=FACE_OUTER_BOUND('',#1684,.T.);
#1227=FACE_OUTER_BOUND('',#1685,.T.);
#1228=FACE_OUTER_BOUND('',#1693,.T.);
#1229=FACE_OUTER_BOUND('',#1695,.T.);
#1230=FACE_OUTER_BOUND('',#1696,.T.);
#1231=FACE_OUTER_BOUND('',#1697,.T.);
#1232=FACE_OUTER_BOUND('',#1698,.T.);
#1233=FACE_OUTER_BOUND('',#1699,.T.);
#1234=FACE_OUTER_BOUND('',#1700,.T.);
#1235=FACE_OUTER_BOUND('',#1702,.T.);
#1236=FACE_OUTER_BOUND('',#1703,.T.);
#1237=FACE_OUTER_BOUND('',#1704,.T.);
#1238=FACE_OUTER_BOUND('',#1710,.T.);
#1239=FACE_OUTER_BOUND('',#1716,.T.);
#1240=FACE_OUTER_BOUND('',#1717,.T.);
#1241=FACE_OUTER_BOUND('',#1718,.T.);
#1242=FACE_OUTER_BOUND('',#1719,.T.);
#1243=FACE_OUTER_BOUND('',#1720,.T.);
#1244=FACE_OUTER_BOUND('',#1721,.T.);
#1245=FACE_OUTER_BOUND('',#1722,.T.);
#1246=FACE_OUTER_BOUND('',#1723,.T.);
#1247=FACE_OUTER_BOUND('',#1725,.T.);
#1248=FACE_OUTER_BOUND('',#1726,.T.);
#1249=FACE_OUTER_BOUND('',#1728,.T.);
#1250=FACE_OUTER_BOUND('',#1729,.T.);
#1251=FACE_OUTER_BOUND('',#1730,.T.);
#1252=FACE_OUTER_BOUND('',#1731,.T.);
#1253=FACE_OUTER_BOUND('',#1733,.T.);
#1254=FACE_OUTER_BOUND('',#1734,.T.);
#1255=FACE_OUTER_BOUND('',#1735,.T.);
#1256=FACE_OUTER_BOUND('',#1736,.T.);
#1257=FACE_OUTER_BOUND('',#1738,.T.);
#1258=FACE_OUTER_BOUND('',#1739,.T.);
#1259=FACE_OUTER_BOUND('',#1740,.T.);
#1260=FACE_OUTER_BOUND('',#1741,.T.);
#1261=FACE_OUTER_BOUND('',#1742,.T.);
#1262=FACE_OUTER_BOUND('',#1743,.T.);
#1263=FACE_OUTER_BOUND('',#1744,.T.);
#1264=FACE_OUTER_BOUND('',#1745,.T.);
#1265=FACE_OUTER_BOUND('',#1746,.T.);
#1266=FACE_OUTER_BOUND('',#1747,.T.);
#1267=FACE_OUTER_BOUND('',#1748,.T.);
#1268=FACE_OUTER_BOUND('',#1749,.T.);
#1269=FACE_OUTER_BOUND('',#1750,.T.);
#1270=FACE_OUTER_BOUND('',#1751,.T.);
#1271=FACE_OUTER_BOUND('',#1752,.T.);
#1272=FACE_OUTER_BOUND('',#1753,.T.);
#1273=FACE_OUTER_BOUND('',#1754,.T.);
#1274=FACE_OUTER_BOUND('',#1755,.T.);
#1275=FACE_OUTER_BOUND('',#1756,.T.);
#1276=FACE_OUTER_BOUND('',#1757,.T.);
#1277=FACE_OUTER_BOUND('',#1758,.T.);
#1278=FACE_OUTER_BOUND('',#1759,.T.);
#1279=FACE_OUTER_BOUND('',#1760,.T.);
#1280=FACE_OUTER_BOUND('',#1761,.T.);
#1281=FACE_OUTER_BOUND('',#1763,.T.);
#1282=FACE_OUTER_BOUND('',#1764,.T.);
#1283=FACE_OUTER_BOUND('',#1766,.T.);
#1284=FACE_OUTER_BOUND('',#1767,.T.);
#1285=FACE_OUTER_BOUND('',#1769,.T.);
#1286=FACE_OUTER_BOUND('',#1770,.T.);
#1287=FACE_OUTER_BOUND('',#1772,.T.);
#1288=FACE_OUTER_BOUND('',#1773,.T.);
#1289=FACE_OUTER_BOUND('',#1775,.T.);
#1290=FACE_OUTER_BOUND('',#1776,.T.);
#1291=FACE_OUTER_BOUND('',#1777,.T.);
#1292=FACE_OUTER_BOUND('',#1778,.T.);
#1293=FACE_OUTER_BOUND('',#1779,.T.);
#1294=FACE_OUTER_BOUND('',#1780,.T.);
#1295=FACE_OUTER_BOUND('',#1782,.T.);
#1296=FACE_OUTER_BOUND('',#1783,.T.);
#1297=FACE_OUTER_BOUND('',#1784,.T.);
#1298=FACE_OUTER_BOUND('',#1785,.T.);
#1299=FACE_OUTER_BOUND('',#1786,.T.);
#1300=FACE_OUTER_BOUND('',#1787,.T.);
#1301=FACE_OUTER_BOUND('',#1788,.T.);
#1302=FACE_OUTER_BOUND('',#1789,.T.);
#1303=FACE_OUTER_BOUND('',#1790,.T.);
#1304=FACE_OUTER_BOUND('',#1791,.T.);
#1305=FACE_OUTER_BOUND('',#1792,.T.);
#1306=FACE_OUTER_BOUND('',#1793,.T.);
#1307=FACE_OUTER_BOUND('',#1794,.T.);
#1308=FACE_OUTER_BOUND('',#1795,.T.);
#1309=FACE_OUTER_BOUND('',#1796,.T.);
#1310=FACE_OUTER_BOUND('',#1797,.T.);
#1311=FACE_OUTER_BOUND('',#1798,.T.);
#1312=FACE_OUTER_BOUND('',#1799,.T.);
#1313=FACE_OUTER_BOUND('',#1801,.T.);
#1314=FACE_OUTER_BOUND('',#1802,.T.);
#1315=FACE_OUTER_BOUND('',#1804,.T.);
#1316=FACE_OUTER_BOUND('',#1805,.T.);
#1317=FACE_OUTER_BOUND('',#1807,.T.);
#1318=FACE_OUTER_BOUND('',#1808,.T.);
#1319=FACE_OUTER_BOUND('',#1810,.T.);
#1320=FACE_OUTER_BOUND('',#1811,.T.);
#1321=FACE_OUTER_BOUND('',#1813,.T.);
#1322=FACE_OUTER_BOUND('',#1814,.T.);
#1323=FACE_OUTER_BOUND('',#1816,.T.);
#1324=FACE_OUTER_BOUND('',#1818,.T.);
#1325=FACE_OUTER_BOUND('',#1819,.T.);
#1326=FACE_OUTER_BOUND('',#1820,.T.);
#1327=FACE_OUTER_BOUND('',#1821,.T.);
#1328=FACE_OUTER_BOUND('',#1822,.T.);
#1329=FACE_OUTER_BOUND('',#1824,.T.);
#1330=FACE_OUTER_BOUND('',#1826,.T.);
#1331=FACE_OUTER_BOUND('',#1828,.T.);
#1332=FACE_OUTER_BOUND('',#1830,.T.);
#1333=FACE_OUTER_BOUND('',#1831,.T.);
#1334=FACE_OUTER_BOUND('',#1832,.T.);
#1335=FACE_OUTER_BOUND('',#1833,.T.);
#1336=FACE_OUTER_BOUND('',#1834,.T.);
#1337=FACE_OUTER_BOUND('',#1835,.T.);
#1338=FACE_OUTER_BOUND('',#1836,.T.);
#1339=FACE_OUTER_BOUND('',#1837,.T.);
#1340=FACE_OUTER_BOUND('',#1838,.T.);
#1341=FACE_OUTER_BOUND('',#1839,.T.);
#1342=FACE_OUTER_BOUND('',#1840,.T.);
#1343=FACE_OUTER_BOUND('',#1841,.T.);
#1344=FACE_OUTER_BOUND('',#1842,.T.);
#1345=FACE_OUTER_BOUND('',#1843,.T.);
#1346=FACE_OUTER_BOUND('',#1845,.T.);
#1347=FACE_OUTER_BOUND('',#1846,.T.);
#1348=FACE_OUTER_BOUND('',#1847,.T.);
#1349=FACE_OUTER_BOUND('',#1848,.T.);
#1350=FACE_OUTER_BOUND('',#1849,.T.);
#1351=FACE_OUTER_BOUND('',#1850,.T.);
#1352=FACE_OUTER_BOUND('',#1851,.T.);
#1353=FACE_OUTER_BOUND('',#1852,.T.);
#1354=FACE_OUTER_BOUND('',#1853,.T.);
#1355=FACE_OUTER_BOUND('',#1854,.T.);
#1356=FACE_OUTER_BOUND('',#1855,.T.);
#1357=FACE_OUTER_BOUND('',#1856,.T.);
#1358=FACE_OUTER_BOUND('',#1857,.T.);
#1359=FACE_OUTER_BOUND('',#1858,.T.);
#1360=FACE_OUTER_BOUND('',#1859,.T.);
#1361=FACE_OUTER_BOUND('',#1860,.T.);
#1362=FACE_OUTER_BOUND('',#1861,.T.);
#1363=FACE_OUTER_BOUND('',#1864,.T.);
#1364=FACE_OUTER_BOUND('',#1866,.T.);
#1365=FACE_OUTER_BOUND('',#1868,.T.);
#1366=FACE_OUTER_BOUND('',#1869,.T.);
#1367=FACE_OUTER_BOUND('',#1870,.T.);
#1368=FACE_OUTER_BOUND('',#1872,.T.);
#1369=FACE_OUTER_BOUND('',#1874,.T.);
#1370=FACE_OUTER_BOUND('',#1875,.T.);
#1371=FACE_OUTER_BOUND('',#1876,.T.);
#1372=FACE_OUTER_BOUND('',#1878,.T.);
#1373=FACE_OUTER_BOUND('',#1880,.T.);
#1374=FACE_OUTER_BOUND('',#1881,.T.);
#1375=FACE_OUTER_BOUND('',#1882,.T.);
#1376=FACE_OUTER_BOUND('',#1884,.T.);
#1377=FACE_OUTER_BOUND('',#1886,.T.);
#1378=FACE_OUTER_BOUND('',#1887,.T.);
#1379=FACE_OUTER_BOUND('',#1888,.T.);
#1380=FACE_OUTER_BOUND('',#1890,.T.);
#1381=FACE_OUTER_BOUND('',#1892,.T.);
#1382=FACE_OUTER_BOUND('',#1893,.T.);
#1383=FACE_OUTER_BOUND('',#1894,.T.);
#1384=FACE_OUTER_BOUND('',#1895,.T.);
#1385=FACE_OUTER_BOUND('',#1897,.T.);
#1386=FACE_OUTER_BOUND('',#1898,.T.);
#1387=FACE_OUTER_BOUND('',#1899,.T.);
#1388=FACE_OUTER_BOUND('',#1900,.T.);
#1389=FACE_OUTER_BOUND('',#1902,.T.);
#1390=FACE_OUTER_BOUND('',#1903,.T.);
#1391=FACE_OUTER_BOUND('',#1905,.T.);
#1392=FACE_OUTER_BOUND('',#1907,.T.);
#1393=FACE_OUTER_BOUND('',#1908,.T.);
#1394=FACE_OUTER_BOUND('',#1909,.T.);
#1395=FACE_OUTER_BOUND('',#1910,.T.);
#1396=FACE_OUTER_BOUND('',#1911,.T.);
#1397=FACE_OUTER_BOUND('',#1913,.T.);
#1398=FACE_OUTER_BOUND('',#1914,.T.);
#1399=FACE_OUTER_BOUND('',#1915,.T.);
#1400=FACE_OUTER_BOUND('',#1917,.T.);
#1401=FACE_OUTER_BOUND('',#1918,.T.);
#1402=FACE_OUTER_BOUND('',#1919,.T.);
#1403=FACE_OUTER_BOUND('',#1921,.T.);
#1404=FACE_OUTER_BOUND('',#1923,.T.);
#1405=FACE_OUTER_BOUND('',#1925,.T.);
#1406=FACE_OUTER_BOUND('',#1926,.T.);
#1407=FACE_OUTER_BOUND('',#1927,.T.);
#1408=FACE_OUTER_BOUND('',#1928,.T.);
#1409=FACE_OUTER_BOUND('',#1929,.T.);
#1410=FACE_OUTER_BOUND('',#1931,.T.);
#1411=FACE_OUTER_BOUND('',#1932,.T.);
#1412=FACE_OUTER_BOUND('',#1933,.T.);
#1413=FACE_OUTER_BOUND('',#1935,.T.);
#1414=FACE_OUTER_BOUND('',#1937,.T.);
#1415=FACE_OUTER_BOUND('',#1938,.T.);
#1416=FACE_OUTER_BOUND('',#1939,.T.);
#1417=FACE_OUTER_BOUND('',#1941,.T.);
#1418=FACE_OUTER_BOUND('',#1943,.T.);
#1419=FACE_OUTER_BOUND('',#1944,.T.);
#1420=FACE_OUTER_BOUND('',#1945,.T.);
#1421=FACE_OUTER_BOUND('',#1946,.T.);
#1422=FACE_OUTER_BOUND('',#1947,.T.);
#1423=FACE_OUTER_BOUND('',#1948,.T.);
#1424=FACE_OUTER_BOUND('',#1949,.T.);
#1425=FACE_OUTER_BOUND('',#1950,.T.);
#1426=FACE_OUTER_BOUND('',#1951,.T.);
#1427=FACE_OUTER_BOUND('',#1952,.T.);
#1428=FACE_OUTER_BOUND('',#1953,.T.);
#1429=FACE_OUTER_BOUND('',#1954,.T.);
#1430=FACE_OUTER_BOUND('',#1955,.T.);
#1431=FACE_OUTER_BOUND('',#1956,.T.);
#1432=FACE_OUTER_BOUND('',#1957,.T.);
#1433=FACE_OUTER_BOUND('',#1959,.T.);
#1434=FACE_OUTER_BOUND('',#1960,.T.);
#1435=FACE_OUTER_BOUND('',#1961,.T.);
#1436=FACE_OUTER_BOUND('',#1962,.T.);
#1437=FACE_OUTER_BOUND('',#1963,.T.);
#1438=FACE_OUTER_BOUND('',#1964,.T.);
#1439=FACE_OUTER_BOUND('',#1965,.T.);
#1440=FACE_OUTER_BOUND('',#1966,.T.);
#1441=FACE_OUTER_BOUND('',#1967,.T.);
#1442=FACE_OUTER_BOUND('',#1968,.T.);
#1443=FACE_OUTER_BOUND('',#1969,.T.);
#1444=FACE_OUTER_BOUND('',#1970,.T.);
#1445=FACE_OUTER_BOUND('',#1971,.T.);
#1446=FACE_OUTER_BOUND('',#1972,.T.);
#1447=FACE_OUTER_BOUND('',#1973,.T.);
#1448=FACE_OUTER_BOUND('',#1974,.T.);
#1449=FACE_OUTER_BOUND('',#1975,.T.);
#1450=FACE_OUTER_BOUND('',#1976,.T.);
#1451=FACE_OUTER_BOUND('',#1978,.T.);
#1452=FACE_OUTER_BOUND('',#1980,.T.);
#1453=FACE_OUTER_BOUND('',#1982,.T.);
#1454=FACE_OUTER_BOUND('',#1983,.T.);
#1455=FACE_OUTER_BOUND('',#1984,.T.);
#1456=FACE_OUTER_BOUND('',#1985,.T.);
#1457=FACE_OUTER_BOUND('',#1986,.T.);
#1458=FACE_OUTER_BOUND('',#1987,.T.);
#1459=FACE_OUTER_BOUND('',#1989,.T.);
#1460=FACE_OUTER_BOUND('',#1990,.T.);
#1461=FACE_OUTER_BOUND('',#1991,.T.);
#1462=FACE_OUTER_BOUND('',#1993,.T.);
#1463=EDGE_LOOP('',(#4095,#4096,#4097,#4098));
#1464=EDGE_LOOP('',(#4099,#4100,#4101,#4102));
#1465=EDGE_LOOP('',(#4103,#4104,#4105,#4106));
#1466=EDGE_LOOP('',(#4107,#4108,#4109,#4110));
#1467=EDGE_LOOP('',(#4111,#4112,#4113,#4114));
#1468=EDGE_LOOP('',(#4115,#4116,#4117,#4118));
#1469=EDGE_LOOP('',(#4119,#4120,#4121,#4122));
#1470=EDGE_LOOP('',(#4123,#4124,#4125,#4126));
#1471=EDGE_LOOP('',(#4127,#4128,#4129,#4130));
#1472=EDGE_LOOP('',(#4131,#4132,#4133,#4134));
#1473=EDGE_LOOP('',(#4135,#4136,#4137,#4138));
#1474=EDGE_LOOP('',(#4139,#4140,#4141,#4142));
#1475=EDGE_LOOP('',(#4143,#4144,#4145,#4146));
#1476=EDGE_LOOP('',(#4147,#4148,#4149,#4150));
#1477=EDGE_LOOP('',(#4151,#4152,#4153,#4154));
#1478=EDGE_LOOP('',(#4155,#4156,#4157,#4158));
#1479=EDGE_LOOP('',(#4159,#4160,#4161,#4162));
#1480=EDGE_LOOP('',(#4163));
#1481=EDGE_LOOP('',(#4164));
#1482=EDGE_LOOP('',(#4165));
#1483=EDGE_LOOP('',(#4166));
#1484=EDGE_LOOP('',(#4167));
#1485=EDGE_LOOP('',(#4168));
#1486=EDGE_LOOP('',(#4169,#4170,#4171,#4172));
#1487=EDGE_LOOP('',(#4173));
#1488=EDGE_LOOP('',(#4174));
#1489=EDGE_LOOP('',(#4175));
#1490=EDGE_LOOP('',(#4176));
#1491=EDGE_LOOP('',(#4177));
#1492=EDGE_LOOP('',(#4178));
#1493=EDGE_LOOP('',(#4179,#4180,#4181,#4182));
#1494=EDGE_LOOP('',(#4183,#4184,#4185,#4186));
#1495=EDGE_LOOP('',(#4187,#4188,#4189,#4190));
#1496=EDGE_LOOP('',(#4191,#4192,#4193,#4194));
#1497=EDGE_LOOP('',(#4195,#4196,#4197,#4198));
#1498=EDGE_LOOP('',(#4199,#4200,#4201,#4202));
#1499=EDGE_LOOP('',(#4203,#4204,#4205,#4206));
#1500=EDGE_LOOP('',(#4207,#4208,#4209,#4210));
#1501=EDGE_LOOP('',(#4211,#4212,#4213,#4214));
#1502=EDGE_LOOP('',(#4215,#4216,#4217,#4218));
#1503=EDGE_LOOP('',(#4219,#4220,#4221,#4222));
#1504=EDGE_LOOP('',(#4223,#4224,#4225,#4226));
#1505=EDGE_LOOP('',(#4227,#4228,#4229,#4230));
#1506=EDGE_LOOP('',(#4231,#4232,#4233,#4234));
#1507=EDGE_LOOP('',(#4235,#4236,#4237,#4238));
#1508=EDGE_LOOP('',(#4239,#4240,#4241,#4242));
#1509=EDGE_LOOP('',(#4243,#4244,#4245,#4246));
#1510=EDGE_LOOP('',(#4247,#4248,#4249,#4250));
#1511=EDGE_LOOP('',(#4251,#4252,#4253,#4254));
#1512=EDGE_LOOP('',(#4255,#4256,#4257,#4258));
#1513=EDGE_LOOP('',(#4259));
#1514=EDGE_LOOP('',(#4260,#4261,#4262,#4263));
#1515=EDGE_LOOP('',(#4264));
#1516=EDGE_LOOP('',(#4265,#4266,#4267,#4268));
#1517=EDGE_LOOP('',(#4269,#4270,#4271,#4272));
#1518=EDGE_LOOP('',(#4273,#4274,#4275,#4276,#4277,#4278,#4279,#4280));
#1519=EDGE_LOOP('',(#4281));
#1520=EDGE_LOOP('',(#4282));
#1521=EDGE_LOOP('',(#4283));
#1522=EDGE_LOOP('',(#4284));
#1523=EDGE_LOOP('',(#4285));
#1524=EDGE_LOOP('',(#4286,#4287,#4288,#4289));
#1525=EDGE_LOOP('',(#4290,#4291,#4292,#4293,#4294,#4295,#4296,#4297));
#1526=EDGE_LOOP('',(#4298));
#1527=EDGE_LOOP('',(#4299));
#1528=EDGE_LOOP('',(#4300));
#1529=EDGE_LOOP('',(#4301));
#1530=EDGE_LOOP('',(#4302));
#1531=EDGE_LOOP('',(#4303,#4304,#4305,#4306));
#1532=EDGE_LOOP('',(#4307,#4308,#4309,#4310));
#1533=EDGE_LOOP('',(#4311,#4312,#4313,#4314));
#1534=EDGE_LOOP('',(#4315));
#1535=EDGE_LOOP('',(#4316));
#1536=EDGE_LOOP('',(#4317,#4318,#4319,#4320));
#1537=EDGE_LOOP('',(#4321,#4322,#4323,#4324));
#1538=EDGE_LOOP('',(#4325,#4326,#4327,#4328));
#1539=EDGE_LOOP('',(#4329,#4330,#4331,#4332));
#1540=EDGE_LOOP('',(#4333,#4334,#4335,#4336));
#1541=EDGE_LOOP('',(#4337));
#1542=EDGE_LOOP('',(#4338));
#1543=EDGE_LOOP('',(#4339,#4340,#4341,#4342));
#1544=EDGE_LOOP('',(#4343,#4344,#4345,#4346));
#1545=EDGE_LOOP('',(#4347));
#1546=EDGE_LOOP('',(#4348));
#1547=EDGE_LOOP('',(#4349));
#1548=EDGE_LOOP('',(#4350));
#1549=EDGE_LOOP('',(#4351));
#1550=EDGE_LOOP('',(#4352));
#1551=EDGE_LOOP('',(#4353));
#1552=EDGE_LOOP('',(#4354));
#1553=EDGE_LOOP('',(#4355));
#1554=EDGE_LOOP('',(#4356));
#1555=EDGE_LOOP('',(#4357));
#1556=EDGE_LOOP('',(#4358));
#1557=EDGE_LOOP('',(#4359,#4360,#4361,#4362));
#1558=EDGE_LOOP('',(#4363,#4364,#4365,#4366));
#1559=EDGE_LOOP('',(#4367,#4368,#4369,#4370));
#1560=EDGE_LOOP('',(#4371,#4372,#4373,#4374));
#1561=EDGE_LOOP('',(#4375,#4376,#4377,#4378));
#1562=EDGE_LOOP('',(#4379));
#1563=EDGE_LOOP('',(#4380));
#1564=EDGE_LOOP('',(#4381,#4382,#4383,#4384));
#1565=EDGE_LOOP('',(#4385,#4386,#4387,#4388));
#1566=EDGE_LOOP('',(#4389));
#1567=EDGE_LOOP('',(#4390));
#1568=EDGE_LOOP('',(#4391));
#1569=EDGE_LOOP('',(#4392));
#1570=EDGE_LOOP('',(#4393));
#1571=EDGE_LOOP('',(#4394));
#1572=EDGE_LOOP('',(#4395));
#1573=EDGE_LOOP('',(#4396));
#1574=EDGE_LOOP('',(#4397));
#1575=EDGE_LOOP('',(#4398));
#1576=EDGE_LOOP('',(#4399));
#1577=EDGE_LOOP('',(#4400));
#1578=EDGE_LOOP('',(#4401,#4402,#4403,#4404));
#1579=EDGE_LOOP('',(#4405,#4406,#4407,#4408));
#1580=EDGE_LOOP('',(#4409,#4410,#4411,#4412));
#1581=EDGE_LOOP('',(#4413,#4414,#4415,#4416));
#1582=EDGE_LOOP('',(#4417,#4418,#4419,#4420));
#1583=EDGE_LOOP('',(#4421,#4422,#4423,#4424));
#1584=EDGE_LOOP('',(#4425,#4426,#4427,#4428));
#1585=EDGE_LOOP('',(#4429,#4430,#4431,#4432));
#1586=EDGE_LOOP('',(#4433));
#1587=EDGE_LOOP('',(#4434,#4435,#4436,#4437));
#1588=EDGE_LOOP('',(#4438));
#1589=EDGE_LOOP('',(#4439,#4440,#4441,#4442));
#1590=EDGE_LOOP('',(#4443,#4444,#4445,#4446));
#1591=EDGE_LOOP('',(#4447,#4448,#4449,#4450,#4451,#4452,#4453,#4454));
#1592=EDGE_LOOP('',(#4455));
#1593=EDGE_LOOP('',(#4456));
#1594=EDGE_LOOP('',(#4457));
#1595=EDGE_LOOP('',(#4458));
#1596=EDGE_LOOP('',(#4459));
#1597=EDGE_LOOP('',(#4460,#4461,#4462,#4463));
#1598=EDGE_LOOP('',(#4464,#4465,#4466,#4467,#4468,#4469,#4470,#4471));
#1599=EDGE_LOOP('',(#4472));
#1600=EDGE_LOOP('',(#4473));
#1601=EDGE_LOOP('',(#4474));
#1602=EDGE_LOOP('',(#4475));
#1603=EDGE_LOOP('',(#4476));
#1604=EDGE_LOOP('',(#4477,#4478,#4479,#4480));
#1605=EDGE_LOOP('',(#4481,#4482,#4483,#4484));
#1606=EDGE_LOOP('',(#4485,#4486,#4487,#4488));
#1607=EDGE_LOOP('',(#4489));
#1608=EDGE_LOOP('',(#4490));
#1609=EDGE_LOOP('',(#4491,#4492,#4493,#4494));
#1610=EDGE_LOOP('',(#4495,#4496,#4497,#4498));
#1611=EDGE_LOOP('',(#4499,#4500,#4501,#4502));
#1612=EDGE_LOOP('',(#4503,#4504,#4505,#4506));
#1613=EDGE_LOOP('',(#4507,#4508,#4509,#4510));
#1614=EDGE_LOOP('',(#4511));
#1615=EDGE_LOOP('',(#4512));
#1616=EDGE_LOOP('',(#4513,#4514,#4515,#4516));
#1617=EDGE_LOOP('',(#4517,#4518,#4519,#4520));
#1618=EDGE_LOOP('',(#4521));
#1619=EDGE_LOOP('',(#4522));
#1620=EDGE_LOOP('',(#4523));
#1621=EDGE_LOOP('',(#4524));
#1622=EDGE_LOOP('',(#4525));
#1623=EDGE_LOOP('',(#4526));
#1624=EDGE_LOOP('',(#4527));
#1625=EDGE_LOOP('',(#4528));
#1626=EDGE_LOOP('',(#4529));
#1627=EDGE_LOOP('',(#4530));
#1628=EDGE_LOOP('',(#4531));
#1629=EDGE_LOOP('',(#4532));
#1630=EDGE_LOOP('',(#4533,#4534,#4535,#4536));
#1631=EDGE_LOOP('',(#4537,#4538,#4539,#4540));
#1632=EDGE_LOOP('',(#4541,#4542,#4543,#4544));
#1633=EDGE_LOOP('',(#4545,#4546,#4547,#4548));
#1634=EDGE_LOOP('',(#4549,#4550,#4551,#4552));
#1635=EDGE_LOOP('',(#4553));
#1636=EDGE_LOOP('',(#4554));
#1637=EDGE_LOOP('',(#4555,#4556,#4557,#4558));
#1638=EDGE_LOOP('',(#4559,#4560,#4561,#4562));
#1639=EDGE_LOOP('',(#4563));
#1640=EDGE_LOOP('',(#4564));
#1641=EDGE_LOOP('',(#4565));
#1642=EDGE_LOOP('',(#4566));
#1643=EDGE_LOOP('',(#4567));
#1644=EDGE_LOOP('',(#4568));
#1645=EDGE_LOOP('',(#4569));
#1646=EDGE_LOOP('',(#4570));
#1647=EDGE_LOOP('',(#4571));
#1648=EDGE_LOOP('',(#4572));
#1649=EDGE_LOOP('',(#4573));
#1650=EDGE_LOOP('',(#4574));
#1651=EDGE_LOOP('',(#4575,#4576,#4577,#4578));
#1652=EDGE_LOOP('',(#4579));
#1653=EDGE_LOOP('',(#4580,#4581,#4582,#4583));
#1654=EDGE_LOOP('',(#4584));
#1655=EDGE_LOOP('',(#4585,#4586,#4587,#4588));
#1656=EDGE_LOOP('',(#4589));
#1657=EDGE_LOOP('',(#4590,#4591,#4592,#4593));
#1658=EDGE_LOOP('',(#4594));
#1659=EDGE_LOOP('',(#4595,#4596,#4597,#4598));
#1660=EDGE_LOOP('',(#4599));
#1661=EDGE_LOOP('',(#4600));
#1662=EDGE_LOOP('',(#4601,#4602,#4603,#4604));
#1663=EDGE_LOOP('',(#4605,#4606,#4607,#4608));
#1664=EDGE_LOOP('',(#4609));
#1665=EDGE_LOOP('',(#4610));
#1666=EDGE_LOOP('',(#4611,#4612,#4613,#4614));
#1667=EDGE_LOOP('',(#4615,#4616,#4617,#4618));
#1668=EDGE_LOOP('',(#4619));
#1669=EDGE_LOOP('',(#4620));
#1670=EDGE_LOOP('',(#4621,#4622,#4623,#4624));
#1671=EDGE_LOOP('',(#4625,#4626,#4627,#4628,#4629,#4630,#4631,#4632,#4633,
#4634,#4635,#4636));
#1672=EDGE_LOOP('',(#4637));
#1673=EDGE_LOOP('',(#4638,#4639,#4640,#4641));
#1674=EDGE_LOOP('',(#4642,#4643,#4644,#4645));
#1675=EDGE_LOOP('',(#4646,#4647,#4648,#4649));
#1676=EDGE_LOOP('',(#4650,#4651,#4652,#4653));
#1677=EDGE_LOOP('',(#4654,#4655,#4656,#4657));
#1678=EDGE_LOOP('',(#4658));
#1679=EDGE_LOOP('',(#4659,#4660,#4661,#4662,#4663,#4664,#4665,#4666));
#1680=EDGE_LOOP('',(#4667,#4668,#4669,#4670));
#1681=EDGE_LOOP('',(#4671,#4672,#4673,#4674));
#1682=EDGE_LOOP('',(#4675,#4676,#4677,#4678));
#1683=EDGE_LOOP('',(#4679,#4680,#4681,#4682));
#1684=EDGE_LOOP('',(#4683,#4684,#4685,#4686,#4687,#4688,#4689,#4690));
#1685=EDGE_LOOP('',(#4691,#4692,#4693,#4694));
#1686=EDGE_LOOP('',(#4695));
#1687=EDGE_LOOP('',(#4696));
#1688=EDGE_LOOP('',(#4697));
#1689=EDGE_LOOP('',(#4698));
#1690=EDGE_LOOP('',(#4699));
#1691=EDGE_LOOP('',(#4700));
#1692=EDGE_LOOP('',(#4701));
#1693=EDGE_LOOP('',(#4702,#4703,#4704,#4705));
#1694=EDGE_LOOP('',(#4706));
#1695=EDGE_LOOP('',(#4707,#4708,#4709,#4710));
#1696=EDGE_LOOP('',(#4711,#4712,#4713,#4714));
#1697=EDGE_LOOP('',(#4715,#4716,#4717,#4718));
#1698=EDGE_LOOP('',(#4719,#4720,#4721,#4722));
#1699=EDGE_LOOP('',(#4723,#4724,#4725,#4726));
#1700=EDGE_LOOP('',(#4727));
#1701=EDGE_LOOP('',(#4728));
#1702=EDGE_LOOP('',(#4729,#4730,#4731,#4732));
#1703=EDGE_LOOP('',(#4733,#4734,#4735,#4736));
#1704=EDGE_LOOP('',(#4737));
#1705=EDGE_LOOP('',(#4738));
#1706=EDGE_LOOP('',(#4739));
#1707=EDGE_LOOP('',(#4740));
#1708=EDGE_LOOP('',(#4741));
#1709=EDGE_LOOP('',(#4742));
#1710=EDGE_LOOP('',(#4743));
#1711=EDGE_LOOP('',(#4744));
#1712=EDGE_LOOP('',(#4745));
#1713=EDGE_LOOP('',(#4746));
#1714=EDGE_LOOP('',(#4747));
#1715=EDGE_LOOP('',(#4748));
#1716=EDGE_LOOP('',(#4749,#4750,#4751,#4752));
#1717=EDGE_LOOP('',(#4753));
#1718=EDGE_LOOP('',(#4754));
#1719=EDGE_LOOP('',(#4755,#4756,#4757,#4758,#4759,#4760));
#1720=EDGE_LOOP('',(#4761,#4762,#4763,#4764,#4765));
#1721=EDGE_LOOP('',(#4766,#4767,#4768,#4769));
#1722=EDGE_LOOP('',(#4770,#4771,#4772,#4773));
#1723=EDGE_LOOP('',(#4774));
#1724=EDGE_LOOP('',(#4775));
#1725=EDGE_LOOP('',(#4776,#4777,#4778,#4779,#4780));
#1726=EDGE_LOOP('',(#4781));
#1727=EDGE_LOOP('',(#4782));
#1728=EDGE_LOOP('',(#4783,#4784,#4785,#4786));
#1729=EDGE_LOOP('',(#4787,#4788,#4789,#4790,#4791,#4792));
#1730=EDGE_LOOP('',(#4793,#4794,#4795,#4796,#4797));
#1731=EDGE_LOOP('',(#4798));
#1732=EDGE_LOOP('',(#4799));
#1733=EDGE_LOOP('',(#4800,#4801,#4802,#4803));
#1734=EDGE_LOOP('',(#4804,#4805,#4806,#4807));
#1735=EDGE_LOOP('',(#4808,#4809,#4810,#4811));
#1736=EDGE_LOOP('',(#4812));
#1737=EDGE_LOOP('',(#4813));
#1738=EDGE_LOOP('',(#4814,#4815,#4816,#4817,#4818));
#1739=EDGE_LOOP('',(#4819,#4820));
#1740=EDGE_LOOP('',(#4821,#4822));
#1741=EDGE_LOOP('',(#4823,#4824));
#1742=EDGE_LOOP('',(#4825,#4826));
#1743=EDGE_LOOP('',(#4827,#4828));
#1744=EDGE_LOOP('',(#4829,#4830));
#1745=EDGE_LOOP('',(#4831,#4832));
#1746=EDGE_LOOP('',(#4833,#4834,#4835,#4836));
#1747=EDGE_LOOP('',(#4837,#4838,#4839,#4840,#4841,#4842,#4843,#4844,#4845,
#4846,#4847,#4848,#4849,#4850,#4851,#4852,#4853,#4854));
#1748=EDGE_LOOP('',(#4855,#4856,#4857,#4858));
#1749=EDGE_LOOP('',(#4859,#4860,#4861,#4862));
#1750=EDGE_LOOP('',(#4863,#4864,#4865,#4866));
#1751=EDGE_LOOP('',(#4867,#4868,#4869,#4870));
#1752=EDGE_LOOP('',(#4871,#4872,#4873,#4874,#4875,#4876));
#1753=EDGE_LOOP('',(#4877,#4878,#4879,#4880));
#1754=EDGE_LOOP('',(#4881,#4882,#4883,#4884));
#1755=EDGE_LOOP('',(#4885,#4886,#4887,#4888));
#1756=EDGE_LOOP('',(#4889,#4890,#4891,#4892));
#1757=EDGE_LOOP('',(#4893,#4894,#4895,#4896));
#1758=EDGE_LOOP('',(#4897,#4898,#4899,#4900,#4901,#4902,#4903,#4904,#4905,
#4906,#4907,#4908,#4909,#4910,#4911,#4912,#4913,#4914));
#1759=EDGE_LOOP('',(#4915,#4916,#4917,#4918));
#1760=EDGE_LOOP('',(#4919,#4920,#4921,#4922));
#1761=EDGE_LOOP('',(#4923));
#1762=EDGE_LOOP('',(#4924));
#1763=EDGE_LOOP('',(#4925,#4926,#4927,#4928));
#1764=EDGE_LOOP('',(#4929));
#1765=EDGE_LOOP('',(#4930));
#1766=EDGE_LOOP('',(#4931,#4932,#4933,#4934));
#1767=EDGE_LOOP('',(#4935));
#1768=EDGE_LOOP('',(#4936));
#1769=EDGE_LOOP('',(#4937,#4938,#4939,#4940));
#1770=EDGE_LOOP('',(#4941));
#1771=EDGE_LOOP('',(#4942));
#1772=EDGE_LOOP('',(#4943,#4944,#4945,#4946));
#1773=EDGE_LOOP('',(#4947));
#1774=EDGE_LOOP('',(#4948));
#1775=EDGE_LOOP('',(#4949,#4950,#4951,#4952));
#1776=EDGE_LOOP('',(#4953));
#1777=EDGE_LOOP('',(#4954,#4955,#4956,#4957));
#1778=EDGE_LOOP('',(#4958,#4959,#4960,#4961));
#1779=EDGE_LOOP('',(#4962,#4963,#4964,#4965));
#1780=EDGE_LOOP('',(#4966));
#1781=EDGE_LOOP('',(#4967));
#1782=EDGE_LOOP('',(#4968,#4969,#4970,#4971));
#1783=EDGE_LOOP('',(#4972,#4973,#4974,#4975));
#1784=EDGE_LOOP('',(#4976,#4977,#4978,#4979));
#1785=EDGE_LOOP('',(#4980));
#1786=EDGE_LOOP('',(#4981,#4982,#4983,#4984));
#1787=EDGE_LOOP('',(#4985,#4986,#4987,#4988));
#1788=EDGE_LOOP('',(#4989,#4990,#4991,#4992));
#1789=EDGE_LOOP('',(#4993,#4994,#4995,#4996));
#1790=EDGE_LOOP('',(#4997,#4998,#4999,#5000));
#1791=EDGE_LOOP('',(#5001,#5002,#5003,#5004));
#1792=EDGE_LOOP('',(#5005,#5006,#5007,#5008,#5009,#5010));
#1793=EDGE_LOOP('',(#5011,#5012,#5013,#5014,#5015,#5016));
#1794=EDGE_LOOP('',(#5017,#5018,#5019,#5020));
#1795=EDGE_LOOP('',(#5021,#5022,#5023,#5024));
#1796=EDGE_LOOP('',(#5025,#5026,#5027,#5028));
#1797=EDGE_LOOP('',(#5029,#5030,#5031,#5032));
#1798=EDGE_LOOP('',(#5033,#5034,#5035,#5036));
#1799=EDGE_LOOP('',(#5037));
#1800=EDGE_LOOP('',(#5038));
#1801=EDGE_LOOP('',(#5039,#5040,#5041,#5042));
#1802=EDGE_LOOP('',(#5043));
#1803=EDGE_LOOP('',(#5044));
#1804=EDGE_LOOP('',(#5045,#5046,#5047,#5048));
#1805=EDGE_LOOP('',(#5049));
#1806=EDGE_LOOP('',(#5050));
#1807=EDGE_LOOP('',(#5051,#5052,#5053,#5054));
#1808=EDGE_LOOP('',(#5055));
#1809=EDGE_LOOP('',(#5056));
#1810=EDGE_LOOP('',(#5057,#5058,#5059,#5060));
#1811=EDGE_LOOP('',(#5061));
#1812=EDGE_LOOP('',(#5062));
#1813=EDGE_LOOP('',(#5063,#5064,#5065,#5066));
#1814=EDGE_LOOP('',(#5067));
#1815=EDGE_LOOP('',(#5068));
#1816=EDGE_LOOP('',(#5069,#5070,#5071,#5072));
#1817=EDGE_LOOP('',(#5073,#5074,#5075,#5076));
#1818=EDGE_LOOP('',(#5077,#5078,#5079,#5080));
#1819=EDGE_LOOP('',(#5081,#5082,#5083,#5084));
#1820=EDGE_LOOP('',(#5085,#5086,#5087,#5088));
#1821=EDGE_LOOP('',(#5089,#5090,#5091,#5092));
#1822=EDGE_LOOP('',(#5093));
#1823=EDGE_LOOP('',(#5094));
#1824=EDGE_LOOP('',(#5095,#5096,#5097,#5098));
#1825=EDGE_LOOP('',(#5099,#5100,#5101,#5102));
#1826=EDGE_LOOP('',(#5103));
#1827=EDGE_LOOP('',(#5104));
#1828=EDGE_LOOP('',(#5105,#5106,#5107,#5108));
#1829=EDGE_LOOP('',(#5109,#5110,#5111,#5112));
#1830=EDGE_LOOP('',(#5113,#5114,#5115,#5116));
#1831=EDGE_LOOP('',(#5117,#5118,#5119,#5120));
#1832=EDGE_LOOP('',(#5121,#5122,#5123,#5124));
#1833=EDGE_LOOP('',(#5125,#5126,#5127,#5128));
#1834=EDGE_LOOP('',(#5129,#5130,#5131,#5132));
#1835=EDGE_LOOP('',(#5133,#5134,#5135,#5136));
#1836=EDGE_LOOP('',(#5137,#5138,#5139,#5140,#5141,#5142));
#1837=EDGE_LOOP('',(#5143,#5144,#5145,#5146,#5147,#5148));
#1838=EDGE_LOOP('',(#5149));
#1839=EDGE_LOOP('',(#5150));
#1840=EDGE_LOOP('',(#5151,#5152,#5153,#5154));
#1841=EDGE_LOOP('',(#5155,#5156,#5157,#5158));
#1842=EDGE_LOOP('',(#5159,#5160,#5161,#5162));
#1843=EDGE_LOOP('',(#5163));
#1844=EDGE_LOOP('',(#5164));
#1845=EDGE_LOOP('',(#5165,#5166,#5167,#5168));
#1846=EDGE_LOOP('',(#5169,#5170,#5171,#5172));
#1847=EDGE_LOOP('',(#5173,#5174,#5175,#5176));
#1848=EDGE_LOOP('',(#5177));
#1849=EDGE_LOOP('',(#5178,#5179,#5180,#5181));
#1850=EDGE_LOOP('',(#5182));
#1851=EDGE_LOOP('',(#5183,#5184,#5185,#5186));
#1852=EDGE_LOOP('',(#5187,#5188,#5189,#5190));
#1853=EDGE_LOOP('',(#5191,#5192,#5193,#5194));
#1854=EDGE_LOOP('',(#5195,#5196,#5197,#5198));
#1855=EDGE_LOOP('',(#5199,#5200,#5201,#5202));
#1856=EDGE_LOOP('',(#5203,#5204,#5205,#5206));
#1857=EDGE_LOOP('',(#5207,#5208,#5209,#5210));
#1858=EDGE_LOOP('',(#5211,#5212,#5213,#5214));
#1859=EDGE_LOOP('',(#5215,#5216,#5217,#5218));
#1860=EDGE_LOOP('',(#5219,#5220,#5221,#5222));
#1861=EDGE_LOOP('',(#5223,#5224,#5225,#5226));
#1862=EDGE_LOOP('',(#5227,#5228,#5229,#5230));
#1863=EDGE_LOOP('',(#5231,#5232,#5233,#5234));
#1864=EDGE_LOOP('',(#5235));
#1865=EDGE_LOOP('',(#5236));
#1866=EDGE_LOOP('',(#5237));
#1867=EDGE_LOOP('',(#5238));
#1868=EDGE_LOOP('',(#5239,#5240,#5241,#5242));
#1869=EDGE_LOOP('',(#5243,#5244,#5245,#5246));
#1870=EDGE_LOOP('',(#5247));
#1871=EDGE_LOOP('',(#5248));
#1872=EDGE_LOOP('',(#5249));
#1873=EDGE_LOOP('',(#5250));
#1874=EDGE_LOOP('',(#5251,#5252,#5253,#5254));
#1875=EDGE_LOOP('',(#5255,#5256,#5257,#5258));
#1876=EDGE_LOOP('',(#5259));
#1877=EDGE_LOOP('',(#5260));
#1878=EDGE_LOOP('',(#5261));
#1879=EDGE_LOOP('',(#5262));
#1880=EDGE_LOOP('',(#5263,#5264,#5265,#5266));
#1881=EDGE_LOOP('',(#5267,#5268,#5269,#5270));
#1882=EDGE_LOOP('',(#5271));
#1883=EDGE_LOOP('',(#5272));
#1884=EDGE_LOOP('',(#5273));
#1885=EDGE_LOOP('',(#5274));
#1886=EDGE_LOOP('',(#5275,#5276,#5277,#5278));
#1887=EDGE_LOOP('',(#5279,#5280,#5281,#5282));
#1888=EDGE_LOOP('',(#5283));
#1889=EDGE_LOOP('',(#5284));
#1890=EDGE_LOOP('',(#5285));
#1891=EDGE_LOOP('',(#5286));
#1892=EDGE_LOOP('',(#5287,#5288,#5289,#5290));
#1893=EDGE_LOOP('',(#5291,#5292,#5293,#5294));
#1894=EDGE_LOOP('',(#5295,#5296,#5297,#5298));
#1895=EDGE_LOOP('',(#5299));
#1896=EDGE_LOOP('',(#5300,#5301,#5302,#5303));
#1897=EDGE_LOOP('',(#5304,#5305,#5306,#5307));
#1898=EDGE_LOOP('',(#5308,#5309,#5310,#5311));
#1899=EDGE_LOOP('',(#5312,#5313,#5314,#5315));
#1900=EDGE_LOOP('',(#5316));
#1901=EDGE_LOOP('',(#5317,#5318,#5319,#5320));
#1902=EDGE_LOOP('',(#5321,#5322,#5323,#5324));
#1903=EDGE_LOOP('',(#5325));
#1904=EDGE_LOOP('',(#5326));
#1905=EDGE_LOOP('',(#5327));
#1906=EDGE_LOOP('',(#5328));
#1907=EDGE_LOOP('',(#5329,#5330,#5331,#5332));
#1908=EDGE_LOOP('',(#5333,#5334,#5335,#5336));
#1909=EDGE_LOOP('',(#5337,#5338,#5339,#5340));
#1910=EDGE_LOOP('',(#5341,#5342,#5343,#5344));
#1911=EDGE_LOOP('',(#5345));
#1912=EDGE_LOOP('',(#5346,#5347,#5348,#5349));
#1913=EDGE_LOOP('',(#5350,#5351,#5352,#5353));
#1914=EDGE_LOOP('',(#5354,#5355,#5356,#5357));
#1915=EDGE_LOOP('',(#5358,#5359,#5360,#5361));
#1916=EDGE_LOOP('',(#5362));
#1917=EDGE_LOOP('',(#5363,#5364,#5365,#5366));
#1918=EDGE_LOOP('',(#5367,#5368,#5369,#5370));
#1919=EDGE_LOOP('',(#5371,#5372,#5373,#5374));
#1920=EDGE_LOOP('',(#5375));
#1921=EDGE_LOOP('',(#5376,#5377,#5378,#5379));
#1922=EDGE_LOOP('',(#5380,#5381,#5382,#5383));
#1923=EDGE_LOOP('',(#5384));
#1924=EDGE_LOOP('',(#5385,#5386,#5387,#5388));
#1925=EDGE_LOOP('',(#5389,#5390,#5391,#5392));
#1926=EDGE_LOOP('',(#5393));
#1927=EDGE_LOOP('',(#5394,#5395,#5396,#5397));
#1928=EDGE_LOOP('',(#5398));
#1929=EDGE_LOOP('',(#5399));
#1930=EDGE_LOOP('',(#5400));
#1931=EDGE_LOOP('',(#5401,#5402,#5403,#5404));
#1932=EDGE_LOOP('',(#5405,#5406,#5407,#5408));
#1933=EDGE_LOOP('',(#5409));
#1934=EDGE_LOOP('',(#5410));
#1935=EDGE_LOOP('',(#5411));
#1936=EDGE_LOOP('',(#5412));
#1937=EDGE_LOOP('',(#5413,#5414,#5415,#5416));
#1938=EDGE_LOOP('',(#5417,#5418,#5419,#5420));
#1939=EDGE_LOOP('',(#5421));
#1940=EDGE_LOOP('',(#5422));
#1941=EDGE_LOOP('',(#5423));
#1942=EDGE_LOOP('',(#5424));
#1943=EDGE_LOOP('',(#5425,#5426,#5427,#5428,#5429,#5430,#5431,#5432));
#1944=EDGE_LOOP('',(#5433,#5434,#5435,#5436));
#1945=EDGE_LOOP('',(#5437,#5438,#5439,#5440));
#1946=EDGE_LOOP('',(#5441,#5442,#5443,#5444));
#1947=EDGE_LOOP('',(#5445,#5446,#5447,#5448));
#1948=EDGE_LOOP('',(#5449,#5450,#5451,#5452,#5453,#5454,#5455,#5456));
#1949=EDGE_LOOP('',(#5457,#5458,#5459,#5460));
#1950=EDGE_LOOP('',(#5461,#5462,#5463,#5464));
#1951=EDGE_LOOP('',(#5465,#5466,#5467,#5468));
#1952=EDGE_LOOP('',(#5469,#5470,#5471,#5472));
#1953=EDGE_LOOP('',(#5473));
#1954=EDGE_LOOP('',(#5474,#5475,#5476,#5477));
#1955=EDGE_LOOP('',(#5478,#5479,#5480,#5481));
#1956=EDGE_LOOP('',(#5482,#5483,#5484,#5485));
#1957=EDGE_LOOP('',(#5486));
#1958=EDGE_LOOP('',(#5487));
#1959=EDGE_LOOP('',(#5488,#5489,#5490,#5491));
#1960=EDGE_LOOP('',(#5492,#5493,#5494,#5495));
#1961=EDGE_LOOP('',(#5496,#5497,#5498,#5499));
#1962=EDGE_LOOP('',(#5500));
#1963=EDGE_LOOP('',(#5501,#5502,#5503,#5504));
#1964=EDGE_LOOP('',(#5505,#5506,#5507,#5508));
#1965=EDGE_LOOP('',(#5509,#5510,#5511,#5512));
#1966=EDGE_LOOP('',(#5513,#5514,#5515,#5516));
#1967=EDGE_LOOP('',(#5517,#5518,#5519,#5520));
#1968=EDGE_LOOP('',(#5521,#5522,#5523,#5524));
#1969=EDGE_LOOP('',(#5525,#5526,#5527,#5528,#5529,#5530));
#1970=EDGE_LOOP('',(#5531,#5532,#5533,#5534,#5535,#5536));
#1971=EDGE_LOOP('',(#5537,#5538,#5539,#5540));
#1972=EDGE_LOOP('',(#5541,#5542,#5543,#5544));
#1973=EDGE_LOOP('',(#5545,#5546,#5547,#5548));
#1974=EDGE_LOOP('',(#5549,#5550,#5551,#5552));
#1975=EDGE_LOOP('',(#5553,#5554,#5555,#5556));
#1976=EDGE_LOOP('',(#5557,#5558,#5559,#5560));
#1977=EDGE_LOOP('',(#5561));
#1978=EDGE_LOOP('',(#5562,#5563,#5564,#5565));
#1979=EDGE_LOOP('',(#5566));
#1980=EDGE_LOOP('',(#5567));
#1981=EDGE_LOOP('',(#5568));
#1982=EDGE_LOOP('',(#5569,#5570,#5571,#5572));
#1983=EDGE_LOOP('',(#5573));
#1984=EDGE_LOOP('',(#5574,#5575,#5576,#5577));
#1985=EDGE_LOOP('',(#5578));
#1986=EDGE_LOOP('',(#5579,#5580,#5581,#5582));
#1987=EDGE_LOOP('',(#5583));
#1988=EDGE_LOOP('',(#5584));
#1989=EDGE_LOOP('',(#5585,#5586,#5587,#5588));
#1990=EDGE_LOOP('',(#5589,#5590,#5591,#5592));
#1991=EDGE_LOOP('',(#5593));
#1992=EDGE_LOOP('',(#5594));
#1993=EDGE_LOOP('',(#5595));
#1994=EDGE_LOOP('',(#5596));
#1995=LINE('',#9426,#2417);
#1996=LINE('',#9428,#2418);
#1997=LINE('',#9430,#2419);
#1998=LINE('',#9431,#2420);
#1999=LINE('',#9434,#2421);
#2000=LINE('',#9436,#2422);
#2001=LINE('',#9437,#2423);
#2002=LINE('',#9440,#2424);
#2003=LINE('',#9442,#2425);
#2004=LINE('',#9443,#2426);
#2005=LINE('',#9445,#2427);
#2006=LINE('',#9446,#2428);
#2007=LINE('',#9452,#2429);
#2008=LINE('',#9458,#2430);
#2009=LINE('',#9464,#2431);
#2010=LINE('',#9470,#2432);
#2011=LINE('',#9476,#2433);
#2012=LINE('',#9482,#2434);
#2013=LINE('',#9487,#2435);
#2014=LINE('',#9489,#2436);
#2015=LINE('',#9491,#2437);
#2016=LINE('',#9492,#2438);
#2017=LINE('',#9495,#2439);
#2018=LINE('',#9497,#2440);
#2019=LINE('',#9498,#2441);
#2020=LINE('',#9501,#2442);
#2021=LINE('',#9503,#2443);
#2022=LINE('',#9504,#2444);
#2023=LINE('',#9506,#2445);
#2024=LINE('',#9507,#2446);
#2025=LINE('',#9514,#2447);
#2026=LINE('',#9516,#2448);
#2027=LINE('',#9518,#2449);
#2028=LINE('',#9519,#2450);
#2029=LINE('',#9522,#2451);
#2030=LINE('',#9524,#2452);
#2031=LINE('',#9525,#2453);
#2032=LINE('',#9528,#2454);
#2033=LINE('',#9530,#2455);
#2034=LINE('',#9531,#2456);
#2035=LINE('',#9533,#2457);
#2036=LINE('',#9534,#2458);
#2037=LINE('',#9541,#2459);
#2038=LINE('',#9543,#2460);
#2039=LINE('',#9545,#2461);
#2040=LINE('',#9546,#2462);
#2041=LINE('',#9549,#2463);
#2042=LINE('',#9551,#2464);
#2043=LINE('',#9552,#2465);
#2044=LINE('',#9555,#2466);
#2045=LINE('',#9557,#2467);
#2046=LINE('',#9558,#2468);
#2047=LINE('',#9560,#2469);
#2048=LINE('',#9561,#2470);
#2049=LINE('',#9569,#2471);
#2050=LINE('',#9575,#2472);
#2051=LINE('',#9581,#2473);
#2052=LINE('',#9587,#2474);
#2053=LINE('',#9593,#2475);
#2054=LINE('',#9599,#2476);
#2055=LINE('',#9605,#2477);
#2056=LINE('',#9610,#2478);
#2057=LINE('',#9612,#2479);
#2058=LINE('',#9614,#2480);
#2059=LINE('',#9615,#2481);
#2060=LINE('',#9619,#2482);
#2061=LINE('',#9621,#2483);
#2062=LINE('',#9623,#2484);
#2063=LINE('',#9624,#2485);
#2064=LINE('',#9627,#2486);
#2065=LINE('',#9629,#2487);
#2066=LINE('',#9630,#2488);
#2067=LINE('',#9633,#2489);
#2068=LINE('',#9635,#2490);
#2069=LINE('',#9636,#2491);
#2070=LINE('',#9639,#2492);
#2071=LINE('',#9641,#2493);
#2072=LINE('',#9642,#2494);
#2073=LINE('',#9643,#2495);
#2074=LINE('',#9646,#2496);
#2075=LINE('',#9647,#2497);
#2076=LINE('',#9650,#2498);
#2077=LINE('',#9651,#2499);
#2078=LINE('',#9652,#2500);
#2079=LINE('',#9654,#2501);
#2080=LINE('',#9662,#2502);
#2081=LINE('',#9668,#2503);
#2082=LINE('',#9674,#2504);
#2083=LINE('',#9680,#2505);
#2084=LINE('',#9686,#2506);
#2085=LINE('',#9693,#2507);
#2086=LINE('',#9699,#2508);
#2087=LINE('',#9708,#2509);
#2088=LINE('',#9714,#2510);
#2089=LINE('',#9720,#2511);
#2090=LINE('',#9726,#2512);
#2091=LINE('',#9732,#2513);
#2092=LINE('',#9740,#2514);
#2093=LINE('',#9745,#2515);
#2094=LINE('',#9754,#2516);
#2095=LINE('',#9760,#2517);
#2096=LINE('',#9766,#2518);
#2097=LINE('',#9772,#2519);
#2098=LINE('',#9778,#2520);
#2099=LINE('',#9784,#2521);
#2100=LINE('',#9790,#2522);
#2101=LINE('',#9795,#2523);
#2102=LINE('',#9797,#2524);
#2103=LINE('',#9799,#2525);
#2104=LINE('',#9800,#2526);
#2105=LINE('',#9804,#2527);
#2106=LINE('',#9806,#2528);
#2107=LINE('',#9808,#2529);
#2108=LINE('',#9809,#2530);
#2109=LINE('',#9812,#2531);
#2110=LINE('',#9814,#2532);
#2111=LINE('',#9815,#2533);
#2112=LINE('',#9818,#2534);
#2113=LINE('',#9820,#2535);
#2114=LINE('',#9821,#2536);
#2115=LINE('',#9824,#2537);
#2116=LINE('',#9826,#2538);
#2117=LINE('',#9827,#2539);
#2118=LINE('',#9828,#2540);
#2119=LINE('',#9831,#2541);
#2120=LINE('',#9832,#2542);
#2121=LINE('',#9835,#2543);
#2122=LINE('',#9836,#2544);
#2123=LINE('',#9837,#2545);
#2124=LINE('',#9839,#2546);
#2125=LINE('',#9847,#2547);
#2126=LINE('',#9853,#2548);
#2127=LINE('',#9859,#2549);
#2128=LINE('',#9865,#2550);
#2129=LINE('',#9871,#2551);
#2130=LINE('',#9878,#2552);
#2131=LINE('',#9884,#2553);
#2132=LINE('',#9893,#2554);
#2133=LINE('',#9899,#2555);
#2134=LINE('',#9905,#2556);
#2135=LINE('',#9911,#2557);
#2136=LINE('',#9917,#2558);
#2137=LINE('',#9925,#2559);
#2138=LINE('',#9930,#2560);
#2139=LINE('',#9939,#2561);
#2140=LINE('',#9946,#2562);
#2141=LINE('',#9953,#2563);
#2142=LINE('',#9960,#2564);
#2143=LINE('',#9967,#2565);
#2144=LINE('',#9975,#2566);
#2145=LINE('',#9980,#2567);
#2146=LINE('',#9988,#2568);
#2147=LINE('',#9993,#2569);
#2148=LINE('',#10001,#2570);
#2149=LINE('',#10005,#2571);
#2150=LINE('',#10007,#2572);
#2151=LINE('',#10009,#2573);
#2152=LINE('',#10011,#2574);
#2153=LINE('',#10013,#2575);
#2154=LINE('',#10015,#2576);
#2155=LINE('',#10017,#2577);
#2156=LINE('',#10019,#2578);
#2157=LINE('',#10021,#2579);
#2158=LINE('',#10023,#2580);
#2159=LINE('',#10025,#2581);
#2160=LINE('',#10026,#2582);
#2161=LINE('',#10030,#2583);
#2162=LINE('',#10031,#2584);
#2163=LINE('',#10032,#2585);
#2164=LINE('',#10036,#2586);
#2165=LINE('',#10037,#2587);
#2166=LINE('',#10038,#2588);
#2167=LINE('',#10041,#2589);
#2168=LINE('',#10043,#2590);
#2169=LINE('',#10044,#2591);
#2170=LINE('',#10047,#2592);
#2171=LINE('',#10048,#2593);
#2172=LINE('',#10051,#2594);
#2173=LINE('',#10052,#2595);
#2174=LINE('',#10054,#2596);
#2175=LINE('',#10055,#2597);
#2176=LINE('',#10059,#2598);
#2177=LINE('',#10061,#2599);
#2178=LINE('',#10062,#2600);
#2179=LINE('',#10065,#2601);
#2180=LINE('',#10066,#2602);
#2181=LINE('',#10069,#2603);
#2182=LINE('',#10070,#2604);
#2183=LINE('',#10072,#2605);
#2184=LINE('',#10073,#2606);
#2185=LINE('',#10081,#2607);
#2186=LINE('',#10087,#2608);
#2187=LINE('',#10093,#2609);
#2188=LINE('',#10099,#2610);
#2189=LINE('',#10105,#2611);
#2190=LINE('',#10113,#2612);
#2191=LINE('',#10118,#2613);
#2192=LINE('',#11507,#2614);
#2193=LINE('',#11513,#2615);
#2194=LINE('',#11517,#2616);
#2195=LINE('',#11523,#2617);
#2196=LINE('',#11528,#2618);
#2197=LINE('',#11543,#2619);
#2198=LINE('',#11552,#2620);
#2199=LINE('',#11556,#2621);
#2200=LINE('',#11560,#2622);
#2201=LINE('',#11563,#2623);
#2202=LINE('',#11699,#2624);
#2203=LINE('',#11952,#2625);
#2204=LINE('',#11994,#2626);
#2205=LINE('',#11999,#2627);
#2206=LINE('',#12008,#2628);
#2207=LINE('',#12013,#2629);
#2208=LINE('',#12026,#2630);
#2209=LINE('',#12030,#2631);
#2210=LINE('',#12034,#2632);
#2211=LINE('',#12041,#2633);
#2212=LINE('',#12045,#2634);
#2213=LINE('',#12049,#2635);
#2214=LINE('',#12054,#2636);
#2215=LINE('',#12056,#2637);
#2216=LINE('',#12058,#2638);
#2217=LINE('',#12059,#2639);
#2218=LINE('',#12062,#2640);
#2219=LINE('',#12064,#2641);
#2220=LINE('',#12065,#2642);
#2221=LINE('',#12068,#2643);
#2222=LINE('',#12070,#2644);
#2223=LINE('',#12071,#2645);
#2224=LINE('',#12074,#2646);
#2225=LINE('',#12076,#2647);
#2226=LINE('',#12077,#2648);
#2227=LINE('',#12080,#2649);
#2228=LINE('',#12082,#2650);
#2229=LINE('',#12083,#2651);
#2230=LINE('',#12085,#2652);
#2231=LINE('',#12086,#2653);
#2232=LINE('',#12096,#2654);
#2233=LINE('',#12098,#2655);
#2234=LINE('',#12099,#2656);
#2235=LINE('',#12102,#2657);
#2236=LINE('',#12104,#2658);
#2237=LINE('',#12105,#2659);
#2238=LINE('',#12110,#2660);
#2239=LINE('',#12111,#2661);
#2240=LINE('',#12113,#2662);
#2241=LINE('',#12114,#2663);
#2242=LINE('',#12124,#2664);
#2243=LINE('',#12131,#2665);
#2244=LINE('',#12138,#2666);
#2245=LINE('',#12145,#2667);
#2246=LINE('',#12152,#2668);
#2247=LINE('',#12157,#2669);
#2248=LINE('',#12164,#2670);
#2249=LINE('',#12167,#2671);
#2250=LINE('',#12170,#2672);
#2251=LINE('',#12172,#2673);
#2252=LINE('',#12173,#2674);
#2253=LINE('',#12179,#2675);
#2254=LINE('',#12181,#2676);
#2255=LINE('',#12182,#2677);
#2256=LINE('',#12191,#2678);
#2257=LINE('',#12196,#2679);
#2258=LINE('',#12203,#2680);
#2259=LINE('',#12205,#2681);
#2260=LINE('',#12207,#2682);
#2261=LINE('',#12208,#2683);
#2262=LINE('',#12211,#2684);
#2263=LINE('',#12213,#2685);
#2264=LINE('',#12214,#2686);
#2265=LINE('',#12217,#2687);
#2266=LINE('',#12219,#2688);
#2267=LINE('',#12220,#2689);
#2268=LINE('',#12223,#2690);
#2269=LINE('',#12225,#2691);
#2270=LINE('',#12226,#2692);
#2271=LINE('',#12229,#2693);
#2272=LINE('',#12231,#2694);
#2273=LINE('',#12232,#2695);
#2274=LINE('',#12234,#2696);
#2275=LINE('',#12235,#2697);
#2276=LINE('',#12247,#2698);
#2277=LINE('',#12251,#2699);
#2278=LINE('',#12255,#2700);
#2279=LINE('',#12262,#2701);
#2280=LINE('',#12264,#2702);
#2281=LINE('',#12271,#2703);
#2282=LINE('',#12278,#2704);
#2283=LINE('',#12284,#2705);
#2284=LINE('',#12286,#2706);
#2285=LINE('',#12288,#2707);
#2286=LINE('',#12289,#2708);
#2287=LINE('',#12294,#2709);
#2288=LINE('',#12295,#2710);
#2289=LINE('',#12298,#2711);
#2290=LINE('',#12300,#2712);
#2291=LINE('',#12301,#2713);
#2292=LINE('',#12303,#2714);
#2293=LINE('',#12309,#2715);
#2294=LINE('',#12311,#2716);
#2295=LINE('',#12313,#2717);
#2296=LINE('',#12314,#2718);
#2297=LINE('',#12319,#2719);
#2298=LINE('',#12320,#2720);
#2299=LINE('',#12323,#2721);
#2300=LINE('',#12325,#2722);
#2301=LINE('',#12326,#2723);
#2302=LINE('',#12328,#2724);
#2303=LINE('',#12335,#2725);
#2304=LINE('',#12344,#2726);
#2305=LINE('',#12350,#2727);
#2306=LINE('',#12359,#2728);
#2307=LINE('',#12365,#2729);
#2308=LINE('',#12374,#2730);
#2309=LINE('',#12380,#2731);
#2310=LINE('',#12389,#2732);
#2311=LINE('',#12395,#2733);
#2312=LINE('',#12403,#2734);
#2313=LINE('',#12405,#2735);
#2314=LINE('',#12407,#2736);
#2315=LINE('',#12408,#2737);
#2316=LINE('',#12411,#2738);
#2317=LINE('',#12413,#2739);
#2318=LINE('',#12414,#2740);
#2319=LINE('',#12417,#2741);
#2320=LINE('',#12419,#2742);
#2321=LINE('',#12420,#2743);
#2322=LINE('',#12431,#2744);
#2323=LINE('',#12435,#2745);
#2324=LINE('',#12442,#2746);
#2325=LINE('',#12451,#2747);
#2326=LINE('',#12456,#2748);
#2327=LINE('',#12458,#2749);
#2328=LINE('',#12460,#2750);
#2329=LINE('',#12461,#2751);
#2330=LINE('',#12464,#2752);
#2331=LINE('',#12466,#2753);
#2332=LINE('',#12467,#2754);
#2333=LINE('',#12470,#2755);
#2334=LINE('',#12472,#2756);
#2335=LINE('',#12473,#2757);
#2336=LINE('',#12483,#2758);
#2337=LINE('',#12487,#2759);
#2338=LINE('',#12491,#2760);
#2339=LINE('',#12494,#2761);
#2340=LINE('',#12497,#2762);
#2341=LINE('',#12498,#2763);
#2342=LINE('',#12501,#2764);
#2343=LINE('',#12502,#2765);
#2344=LINE('',#12507,#2766);
#2345=LINE('',#12515,#2767);
#2346=LINE('',#12522,#2768);
#2347=LINE('',#12531,#2769);
#2348=LINE('',#12537,#2770);
#2349=LINE('',#12546,#2771);
#2350=LINE('',#12552,#2772);
#2351=LINE('',#12560,#2773);
#2352=LINE('',#12562,#2774);
#2353=LINE('',#12564,#2775);
#2354=LINE('',#12566,#2776);
#2355=LINE('',#12568,#2777);
#2356=LINE('',#12570,#2778);
#2357=LINE('',#12572,#2779);
#2358=LINE('',#12573,#2780);
#2359=LINE('',#12576,#2781);
#2360=LINE('',#12578,#2782);
#2361=LINE('',#12579,#2783);
#2362=LINE('',#12582,#2784);
#2363=LINE('',#12583,#2785);
#2364=LINE('',#12586,#2786);
#2365=LINE('',#12587,#2787);
#2366=LINE('',#12590,#2788);
#2367=LINE('',#12591,#2789);
#2368=LINE('',#12594,#2790);
#2369=LINE('',#12596,#2791);
#2370=LINE('',#12598,#2792);
#2371=LINE('',#12599,#2793);
#2372=LINE('',#12601,#2794);
#2373=LINE('',#12603,#2795);
#2374=LINE('',#12605,#2796);
#2375=LINE('',#12614,#2797);
#2376=LINE('',#12618,#2798);
#2377=LINE('',#12622,#2799);
#2378=LINE('',#12629,#2800);
#2379=LINE('',#12633,#2801);
#2380=LINE('',#12637,#2802);
#2381=LINE('',#12642,#2803);
#2382=LINE('',#12644,#2804);
#2383=LINE('',#12646,#2805);
#2384=LINE('',#12647,#2806);
#2385=LINE('',#12650,#2807);
#2386=LINE('',#12652,#2808);
#2387=LINE('',#12653,#2809);
#2388=LINE('',#12656,#2810);
#2389=LINE('',#12658,#2811);
#2390=LINE('',#12659,#2812);
#2391=LINE('',#12662,#2813);
#2392=LINE('',#12664,#2814);
#2393=LINE('',#12665,#2815);
#2394=LINE('',#12668,#2816);
#2395=LINE('',#12670,#2817);
#2396=LINE('',#12671,#2818);
#2397=LINE('',#12673,#2819);
#2398=LINE('',#12674,#2820);
#2399=LINE('',#12739,#2821);
#2400=LINE('',#12744,#2822);
#2401=LINE('',#12746,#2823);
#2402=LINE('',#12748,#2824);
#2403=LINE('',#12749,#2825);
#2404=LINE('',#12752,#2826);
#2405=LINE('',#12754,#2827);
#2406=LINE('',#12755,#2828);
#2407=LINE('',#12758,#2829);
#2408=LINE('',#12760,#2830);
#2409=LINE('',#12761,#2831);
#2410=LINE('',#12763,#2832);
#2411=LINE('',#12764,#2833);
#2412=LINE('',#12776,#2834);
#2413=LINE('',#12782,#2835);
#2414=LINE('',#12787,#2836);
#2415=LINE('',#12795,#2837);
#2416=LINE('',#12801,#2838);
#2417=VECTOR('',#7422,1.);
#2418=VECTOR('',#7423,1.);
#2419=VECTOR('',#7424,1.);
#2420=VECTOR('',#7425,1.);
#2421=VECTOR('',#7428,1.);
#2422=VECTOR('',#7429,1.);
#2423=VECTOR('',#7430,1.);
#2424=VECTOR('',#7433,1.);
#2425=VECTOR('',#7434,1.);
#2426=VECTOR('',#7435,1.);
#2427=VECTOR('',#7438,1.);
#2428=VECTOR('',#7439,1.);
#2429=VECTOR('',#7446,0.21);
#2430=VECTOR('',#7453,0.21);
#2431=VECTOR('',#7460,0.165);
#2432=VECTOR('',#7467,0.165);
#2433=VECTOR('',#7474,0.165);
#2434=VECTOR('',#7481,0.165);
#2435=VECTOR('',#7486,1.);
#2436=VECTOR('',#7487,1.);
#2437=VECTOR('',#7488,1.);
#2438=VECTOR('',#7489,1.);
#2439=VECTOR('',#7492,1.);
#2440=VECTOR('',#7493,1.);
#2441=VECTOR('',#7494,1.);
#2442=VECTOR('',#7497,1.);
#2443=VECTOR('',#7498,1.);
#2444=VECTOR('',#7499,1.);
#2445=VECTOR('',#7502,1.);
#2446=VECTOR('',#7503,1.);
#2447=VECTOR('',#7512,1.);
#2448=VECTOR('',#7513,1.);
#2449=VECTOR('',#7514,1.);
#2450=VECTOR('',#7515,1.);
#2451=VECTOR('',#7518,1.);
#2452=VECTOR('',#7519,1.);
#2453=VECTOR('',#7520,1.);
#2454=VECTOR('',#7523,1.);
#2455=VECTOR('',#7524,1.);
#2456=VECTOR('',#7525,1.);
#2457=VECTOR('',#7528,1.);
#2458=VECTOR('',#7529,1.);
#2459=VECTOR('',#7538,1.);
#2460=VECTOR('',#7539,1.);
#2461=VECTOR('',#7540,1.);
#2462=VECTOR('',#7541,1.);
#2463=VECTOR('',#7544,1.);
#2464=VECTOR('',#7545,1.);
#2465=VECTOR('',#7546,1.);
#2466=VECTOR('',#7549,1.);
#2467=VECTOR('',#7550,1.);
#2468=VECTOR('',#7551,1.);
#2469=VECTOR('',#7554,1.);
#2470=VECTOR('',#7555,1.);
#2471=VECTOR('',#7566,0.225);
#2472=VECTOR('',#7573,0.225);
#2473=VECTOR('',#7580,0.165);
#2474=VECTOR('',#7587,0.165);
#2475=VECTOR('',#7594,0.165);
#2476=VECTOR('',#7601,0.165);
#2477=VECTOR('',#7608,1.6);
#2478=VECTOR('',#7613,1.);
#2479=VECTOR('',#7614,1.);
#2480=VECTOR('',#7615,1.);
#2481=VECTOR('',#7616,1.);
#2482=VECTOR('',#7619,1.);
#2483=VECTOR('',#7620,1.);
#2484=VECTOR('',#7621,1.);
#2485=VECTOR('',#7622,1.);
#2486=VECTOR('',#7625,1.);
#2487=VECTOR('',#7626,1.);
#2488=VECTOR('',#7627,1.);
#2489=VECTOR('',#7630,1.);
#2490=VECTOR('',#7631,1.);
#2491=VECTOR('',#7632,1.);
#2492=VECTOR('',#7635,1.);
#2493=VECTOR('',#7636,1.);
#2494=VECTOR('',#7637,1.);
#2495=VECTOR('',#7638,1.);
#2496=VECTOR('',#7641,1.);
#2497=VECTOR('',#7642,1.);
#2498=VECTOR('',#7645,1.);
#2499=VECTOR('',#7646,1.);
#2500=VECTOR('',#7647,1.);
#2501=VECTOR('',#7650,1.);
#2502=VECTOR('',#7661,0.225);
#2503=VECTOR('',#7668,0.225);
#2504=VECTOR('',#7675,0.225);
#2505=VECTOR('',#7682,0.225);
#2506=VECTOR('',#7689,1.59);
#2507=VECTOR('',#7698,1.005);
#2508=VECTOR('',#7705,2.4);
#2509=VECTOR('',#7718,0.225);
#2510=VECTOR('',#7725,0.225);
#2511=VECTOR('',#7732,0.225);
#2512=VECTOR('',#7739,0.225);
#2513=VECTOR('',#7746,1.59);
#2514=VECTOR('',#7757,1.005);
#2515=VECTOR('',#7762,2.4);
#2516=VECTOR('',#7775,0.225);
#2517=VECTOR('',#7782,0.225);
#2518=VECTOR('',#7789,0.165);
#2519=VECTOR('',#7796,0.165);
#2520=VECTOR('',#7803,0.165);
#2521=VECTOR('',#7810,0.165);
#2522=VECTOR('',#7817,1.6);
#2523=VECTOR('',#7822,1.);
#2524=VECTOR('',#7823,1.);
#2525=VECTOR('',#7824,1.);
#2526=VECTOR('',#7825,1.);
#2527=VECTOR('',#7828,1.);
#2528=VECTOR('',#7829,1.);
#2529=VECTOR('',#7830,1.);
#2530=VECTOR('',#7831,1.);
#2531=VECTOR('',#7834,1.);
#2532=VECTOR('',#7835,1.);
#2533=VECTOR('',#7836,1.);
#2534=VECTOR('',#7839,1.);
#2535=VECTOR('',#7840,1.);
#2536=VECTOR('',#7841,1.);
#2537=VECTOR('',#7844,1.);
#2538=VECTOR('',#7845,1.);
#2539=VECTOR('',#7846,1.);
#2540=VECTOR('',#7847,1.);
#2541=VECTOR('',#7850,1.);
#2542=VECTOR('',#7851,1.);
#2543=VECTOR('',#7854,1.);
#2544=VECTOR('',#7855,1.);
#2545=VECTOR('',#7856,1.);
#2546=VECTOR('',#7859,1.);
#2547=VECTOR('',#7870,0.225);
#2548=VECTOR('',#7877,0.225);
#2549=VECTOR('',#7884,0.225);
#2550=VECTOR('',#7891,0.225);
#2551=VECTOR('',#7898,1.59);
#2552=VECTOR('',#7907,1.005);
#2553=VECTOR('',#7914,2.4);
#2554=VECTOR('',#7927,0.225);
#2555=VECTOR('',#7934,0.225);
#2556=VECTOR('',#7941,0.225);
#2557=VECTOR('',#7948,0.225);
#2558=VECTOR('',#7955,1.59);
#2559=VECTOR('',#7966,1.005);
#2560=VECTOR('',#7971,2.4);
#2561=VECTOR('',#7984,0.165);
#2562=VECTOR('',#7993,0.165);
#2563=VECTOR('',#8002,0.165);
#2564=VECTOR('',#8011,0.165);
#2565=VECTOR('',#8020,1.05);
#2566=VECTOR('',#8031,0.625);
#2567=VECTOR('',#8036,0.5);
#2568=VECTOR('',#8047,0.275);
#2569=VECTOR('',#8052,0.5);
#2570=VECTOR('',#8063,0.275);
#2571=VECTOR('',#8066,1.);
#2572=VECTOR('',#8067,1.);
#2573=VECTOR('',#8068,1.);
#2574=VECTOR('',#8069,1.);
#2575=VECTOR('',#8070,1.);
#2576=VECTOR('',#8071,1.);
#2577=VECTOR('',#8072,1.);
#2578=VECTOR('',#8073,1.);
#2579=VECTOR('',#8074,1.);
#2580=VECTOR('',#8075,1.);
#2581=VECTOR('',#8076,1.);
#2582=VECTOR('',#8077,1.);
#2583=VECTOR('',#8080,1.);
#2584=VECTOR('',#8081,1.);
#2585=VECTOR('',#8082,1.);
#2586=VECTOR('',#8085,1.);
#2587=VECTOR('',#8086,1.);
#2588=VECTOR('',#8087,1.);
#2589=VECTOR('',#8090,1.);
#2590=VECTOR('',#8091,1.);
#2591=VECTOR('',#8092,1.);
#2592=VECTOR('',#8095,1.);
#2593=VECTOR('',#8096,1.);
#2594=VECTOR('',#8099,1.);
#2595=VECTOR('',#8100,1.);
#2596=VECTOR('',#8103,1.);
#2597=VECTOR('',#8104,1.);
#2598=VECTOR('',#8109,1.);
#2599=VECTOR('',#8110,1.);
#2600=VECTOR('',#8111,1.);
#2601=VECTOR('',#8114,1.);
#2602=VECTOR('',#8115,1.);
#2603=VECTOR('',#8118,1.);
#2604=VECTOR('',#8119,1.);
#2605=VECTOR('',#8122,1.);
#2606=VECTOR('',#8123,1.);
#2607=VECTOR('',#8134,0.225);
#2608=VECTOR('',#8141,0.225);
#2609=VECTOR('',#8148,0.225);
#2610=VECTOR('',#8155,0.225);
#2611=VECTOR('',#8162,1.04);
#2612=VECTOR('',#8173,0.625);
#2613=VECTOR('',#8178,1.8);
#2614=VECTOR('',#8213,1.070235);
#2615=VECTOR('',#8220,0.6);
#2616=VECTOR('',#8225,0.63);
#2617=VECTOR('',#8234,1.070235);
#2618=VECTOR('',#8241,0.63);
#2619=VECTOR('',#8260,1.129765);
#2620=VECTOR('',#8271,1.57);
#2621=VECTOR('',#8276,1.6);
#2622=VECTOR('',#8281,1.57);
#2623=VECTOR('',#8286,1.129765);
#2624=VECTOR('',#8333,1.123812);
#2625=VECTOR('',#8402,1.076188);
#2626=VECTOR('',#8431,1.119765);
#2627=VECTOR('',#8438,1.085235);
#2628=VECTOR('',#8449,1.119765);
#2629=VECTOR('',#8456,1.085235);
#2630=VECTOR('',#8477,0.4);
#2631=VECTOR('',#8482,0.425);
#2632=VECTOR('',#8487,0.41);
#2633=VECTOR('',#8496,0.26);
#2634=VECTOR('',#8501,0.25);
#2635=VECTOR('',#8506,0.225);
#2636=VECTOR('',#8511,1.);
#2637=VECTOR('',#8512,1.);
#2638=VECTOR('',#8513,1.);
#2639=VECTOR('',#8514,1.);
#2640=VECTOR('',#8517,1.);
#2641=VECTOR('',#8518,1.);
#2642=VECTOR('',#8519,1.);
#2643=VECTOR('',#8522,1.);
#2644=VECTOR('',#8523,1.);
#2645=VECTOR('',#8524,1.);
#2646=VECTOR('',#8527,1.);
#2647=VECTOR('',#8528,1.);
#2648=VECTOR('',#8529,1.);
#2649=VECTOR('',#8532,1.);
#2650=VECTOR('',#8533,1.);
#2651=VECTOR('',#8534,1.);
#2652=VECTOR('',#8537,1.);
#2653=VECTOR('',#8538,1.);
#2654=VECTOR('',#8551,1.);
#2655=VECTOR('',#8552,1.);
#2656=VECTOR('',#8553,1.);
#2657=VECTOR('',#8556,1.);
#2658=VECTOR('',#8557,1.);
#2659=VECTOR('',#8558,1.);
#2660=VECTOR('',#8563,1.);
#2661=VECTOR('',#8564,1.);
#2662=VECTOR('',#8567,1.);
#2663=VECTOR('',#8568,1.);
#2664=VECTOR('',#8581,1.05);
#2665=VECTOR('',#8590,1.);
#2666=VECTOR('',#8599,1.05);
#2667=VECTOR('',#8608,1.);
#2668=VECTOR('',#8617,1.05);
#2669=VECTOR('',#8624,0.9);
#2670=VECTOR('',#8631,1.);
#2671=VECTOR('',#8634,1.);
#2672=VECTOR('',#8637,1.);
#2673=VECTOR('',#8638,1.);
#2674=VECTOR('',#8639,1.);
#2675=VECTOR('',#8646,1.);
#2676=VECTOR('',#8649,1.);
#2677=VECTOR('',#8650,1.);
#2678=VECTOR('',#8661,0.895);
#2679=VECTOR('',#8668,0.605);
#2680=VECTOR('',#8677,1.);
#2681=VECTOR('',#8678,1.);
#2682=VECTOR('',#8679,1.);
#2683=VECTOR('',#8680,1.);
#2684=VECTOR('',#8683,1.);
#2685=VECTOR('',#8684,1.);
#2686=VECTOR('',#8685,1.);
#2687=VECTOR('',#8688,1.);
#2688=VECTOR('',#8689,1.);
#2689=VECTOR('',#8690,1.);
#2690=VECTOR('',#8693,1.);
#2691=VECTOR('',#8694,1.);
#2692=VECTOR('',#8695,1.);
#2693=VECTOR('',#8698,1.);
#2694=VECTOR('',#8699,1.);
#2695=VECTOR('',#8700,1.);
#2696=VECTOR('',#8703,1.);
#2697=VECTOR('',#8704,1.);
#2698=VECTOR('',#8721,0.325);
#2699=VECTOR('',#8726,0.35);
#2700=VECTOR('',#8731,0.335);
#2701=VECTOR('',#8740,0.21);
#2702=VECTOR('',#8743,0.2);
#2703=VECTOR('',#8752,0.165);
#2704=VECTOR('',#8761,0.165);
#2705=VECTOR('',#8768,1.);
#2706=VECTOR('',#8769,1.);
#2707=VECTOR('',#8770,1.);
#2708=VECTOR('',#8771,1.);
#2709=VECTOR('',#8776,1.);
#2710=VECTOR('',#8777,1.);
#2711=VECTOR('',#8780,1.);
#2712=VECTOR('',#8781,1.);
#2713=VECTOR('',#8782,1.);
#2714=VECTOR('',#8785,1.);
#2715=VECTOR('',#8792,1.);
#2716=VECTOR('',#8793,1.);
#2717=VECTOR('',#8794,1.);
#2718=VECTOR('',#8795,1.);
#2719=VECTOR('',#8800,1.);
#2720=VECTOR('',#8801,1.);
#2721=VECTOR('',#8804,1.);
#2722=VECTOR('',#8805,1.);
#2723=VECTOR('',#8806,1.);
#2724=VECTOR('',#8809,1.);
#2725=VECTOR('',#8818,0.6);
#2726=VECTOR('',#8831,0.605);
#2727=VECTOR('',#8838,0.8);
#2728=VECTOR('',#8851,0.605);
#2729=VECTOR('',#8858,0.8);
#2730=VECTOR('',#8871,0.605);
#2731=VECTOR('',#8878,0.8);
#2732=VECTOR('',#8891,0.605);
#2733=VECTOR('',#8898,0.8);
#2734=VECTOR('',#8909,1.);
#2735=VECTOR('',#8910,1.);
#2736=VECTOR('',#8911,1.);
#2737=VECTOR('',#8912,1.);
#2738=VECTOR('',#8915,1.);
#2739=VECTOR('',#8916,1.);
#2740=VECTOR('',#8917,1.);
#2741=VECTOR('',#8920,1.);
#2742=VECTOR('',#8921,1.);
#2743=VECTOR('',#8922,1.);
#2744=VECTOR('',#8937,1.2);
#2745=VECTOR('',#8942,1.2);
#2746=VECTOR('',#8951,2.);
#2747=VECTOR('',#8964,0.225);
#2748=VECTOR('',#8969,1.);
#2749=VECTOR('',#8970,1.);
#2750=VECTOR('',#8971,1.);
#2751=VECTOR('',#8972,1.);
#2752=VECTOR('',#8975,1.);
#2753=VECTOR('',#8976,1.);
#2754=VECTOR('',#8977,1.);
#2755=VECTOR('',#8980,1.);
#2756=VECTOR('',#8981,1.);
#2757=VECTOR('',#8982,1.);
#2758=VECTOR('',#8995,1.);
#2759=VECTOR('',#8998,1.);
#2760=VECTOR('',#9003,1.);
#2761=VECTOR('',#9006,1.);
#2762=VECTOR('',#9009,1.);
#2763=VECTOR('',#9010,1.);
#2764=VECTOR('',#9013,1.);
#2765=VECTOR('',#9014,1.);
#2766=VECTOR('',#9021,1.2);
#2767=VECTOR('',#9032,0.165);
#2768=VECTOR('',#9041,0.6);
#2769=VECTOR('',#9054,0.225);
#2770=VECTOR('',#9061,1.);
#2771=VECTOR('',#9074,0.225);
#2772=VECTOR('',#9081,1.);
#2773=VECTOR('',#9092,1.);
#2774=VECTOR('',#9093,1.);
#2775=VECTOR('',#9094,1.);
#2776=VECTOR('',#9095,1.);
#2777=VECTOR('',#9096,1.);
#2778=VECTOR('',#9097,1.);
#2779=VECTOR('',#9098,1.);
#2780=VECTOR('',#9099,1.);
#2781=VECTOR('',#9102,1.);
#2782=VECTOR('',#9103,1.);
#2783=VECTOR('',#9104,1.);
#2784=VECTOR('',#9107,1.);
#2785=VECTOR('',#9108,1.);
#2786=VECTOR('',#9111,1.);
#2787=VECTOR('',#9112,1.);
#2788=VECTOR('',#9115,1.);
#2789=VECTOR('',#9116,1.);
#2790=VECTOR('',#9119,1.);
#2791=VECTOR('',#9120,1.);
#2792=VECTOR('',#9121,1.);
#2793=VECTOR('',#9122,1.);
#2794=VECTOR('',#9125,1.);
#2795=VECTOR('',#9128,1.);
#2796=VECTOR('',#9131,1.);
#2797=VECTOR('',#9144,0.325);
#2798=VECTOR('',#9149,0.35);
#2799=VECTOR('',#9154,0.335);
#2800=VECTOR('',#9163,0.21);
#2801=VECTOR('',#9168,0.2);
#2802=VECTOR('',#9173,0.18);
#2803=VECTOR('',#9178,1.);
#2804=VECTOR('',#9179,1.);
#2805=VECTOR('',#9180,1.);
#2806=VECTOR('',#9181,1.);
#2807=VECTOR('',#9184,1.);
#2808=VECTOR('',#9185,1.);
#2809=VECTOR('',#9186,1.);
#2810=VECTOR('',#9189,1.);
#2811=VECTOR('',#9190,1.);
#2812=VECTOR('',#9191,1.);
#2813=VECTOR('',#9194,1.);
#2814=VECTOR('',#9195,1.);
#2815=VECTOR('',#9196,1.);
#2816=VECTOR('',#9199,1.);
#2817=VECTOR('',#9200,1.);
#2818=VECTOR('',#9201,1.);
#2819=VECTOR('',#9204,1.);
#2820=VECTOR('',#9205,1.);
#2821=VECTOR('',#9330,0.425);
#2822=VECTOR('',#9335,1.);
#2823=VECTOR('',#9336,1.);
#2824=VECTOR('',#9337,1.);
#2825=VECTOR('',#9338,1.);
#2826=VECTOR('',#9341,1.);
#2827=VECTOR('',#9342,1.);
#2828=VECTOR('',#9343,1.);
#2829=VECTOR('',#9346,1.);
#2830=VECTOR('',#9347,1.);
#2831=VECTOR('',#9348,1.);
#2832=VECTOR('',#9351,1.);
#2833=VECTOR('',#9352,1.);
#2834=VECTOR('',#9369,0.9);
#2835=VECTOR('',#9376,0.5);
#2836=VECTOR('',#9383,0.6);
#2837=VECTOR('',#9394,0.605);
#2838=VECTOR('',#9401,1.25);
#2839=VERTEX_POINT('',#9424);
#2840=VERTEX_POINT('',#9425);
#2841=VERTEX_POINT('',#9427);
#2842=VERTEX_POINT('',#9429);
#2843=VERTEX_POINT('',#9433);
#2844=VERTEX_POINT('',#9435);
#2845=VERTEX_POINT('',#9439);
#2846=VERTEX_POINT('',#9441);
#2847=VERTEX_POINT('',#9449);
#2848=VERTEX_POINT('',#9451);
#2849=VERTEX_POINT('',#9455);
#2850=VERTEX_POINT('',#9457);
#2851=VERTEX_POINT('',#9461);
#2852=VERTEX_POINT('',#9463);
#2853=VERTEX_POINT('',#9467);
#2854=VERTEX_POINT('',#9469);
#2855=VERTEX_POINT('',#9473);
#2856=VERTEX_POINT('',#9475);
#2857=VERTEX_POINT('',#9479);
#2858=VERTEX_POINT('',#9481);
#2859=VERTEX_POINT('',#9485);
#2860=VERTEX_POINT('',#9486);
#2861=VERTEX_POINT('',#9488);
#2862=VERTEX_POINT('',#9490);
#2863=VERTEX_POINT('',#9494);
#2864=VERTEX_POINT('',#9496);
#2865=VERTEX_POINT('',#9500);
#2866=VERTEX_POINT('',#9502);
#2867=VERTEX_POINT('',#9512);
#2868=VERTEX_POINT('',#9513);
#2869=VERTEX_POINT('',#9515);
#2870=VERTEX_POINT('',#9517);
#2871=VERTEX_POINT('',#9521);
#2872=VERTEX_POINT('',#9523);
#2873=VERTEX_POINT('',#9527);
#2874=VERTEX_POINT('',#9529);
#2875=VERTEX_POINT('',#9539);
#2876=VERTEX_POINT('',#9540);
#2877=VERTEX_POINT('',#9542);
#2878=VERTEX_POINT('',#9544);
#2879=VERTEX_POINT('',#9548);
#2880=VERTEX_POINT('',#9550);
#2881=VERTEX_POINT('',#9554);
#2882=VERTEX_POINT('',#9556);
#2883=VERTEX_POINT('',#9566);
#2884=VERTEX_POINT('',#9568);
#2885=VERTEX_POINT('',#9572);
#2886=VERTEX_POINT('',#9574);
#2887=VERTEX_POINT('',#9578);
#2888=VERTEX_POINT('',#9580);
#2889=VERTEX_POINT('',#9584);
#2890=VERTEX_POINT('',#9586);
#2891=VERTEX_POINT('',#9590);
#2892=VERTEX_POINT('',#9592);
#2893=VERTEX_POINT('',#9596);
#2894=VERTEX_POINT('',#9598);
#2895=VERTEX_POINT('',#9602);
#2896=VERTEX_POINT('',#9604);
#2897=VERTEX_POINT('',#9608);
#2898=VERTEX_POINT('',#9609);
#2899=VERTEX_POINT('',#9611);
#2900=VERTEX_POINT('',#9613);
#2901=VERTEX_POINT('',#9617);
#2902=VERTEX_POINT('',#9618);
#2903=VERTEX_POINT('',#9620);
#2904=VERTEX_POINT('',#9622);
#2905=VERTEX_POINT('',#9626);
#2906=VERTEX_POINT('',#9628);
#2907=VERTEX_POINT('',#9632);
#2908=VERTEX_POINT('',#9634);
#2909=VERTEX_POINT('',#9638);
#2910=VERTEX_POINT('',#9640);
#2911=VERTEX_POINT('',#9645);
#2912=VERTEX_POINT('',#9649);
#2913=VERTEX_POINT('',#9659);
#2914=VERTEX_POINT('',#9661);
#2915=VERTEX_POINT('',#9665);
#2916=VERTEX_POINT('',#9667);
#2917=VERTEX_POINT('',#9671);
#2918=VERTEX_POINT('',#9673);
#2919=VERTEX_POINT('',#9677);
#2920=VERTEX_POINT('',#9679);
#2921=VERTEX_POINT('',#9683);
#2922=VERTEX_POINT('',#9685);
#2923=VERTEX_POINT('',#9689);
#2924=VERTEX_POINT('',#9692);
#2925=VERTEX_POINT('',#9696);
#2926=VERTEX_POINT('',#9698);
#2927=VERTEX_POINT('',#9705);
#2928=VERTEX_POINT('',#9707);
#2929=VERTEX_POINT('',#9711);
#2930=VERTEX_POINT('',#9713);
#2931=VERTEX_POINT('',#9717);
#2932=VERTEX_POINT('',#9719);
#2933=VERTEX_POINT('',#9723);
#2934=VERTEX_POINT('',#9725);
#2935=VERTEX_POINT('',#9729);
#2936=VERTEX_POINT('',#9731);
#2937=VERTEX_POINT('',#9735);
#2938=VERTEX_POINT('',#9738);
#2939=VERTEX_POINT('',#9742);
#2940=VERTEX_POINT('',#9744);
#2941=VERTEX_POINT('',#9751);
#2942=VERTEX_POINT('',#9753);
#2943=VERTEX_POINT('',#9757);
#2944=VERTEX_POINT('',#9759);
#2945=VERTEX_POINT('',#9763);
#2946=VERTEX_POINT('',#9765);
#2947=VERTEX_POINT('',#9769);
#2948=VERTEX_POINT('',#9771);
#2949=VERTEX_POINT('',#9775);
#2950=VERTEX_POINT('',#9777);
#2951=VERTEX_POINT('',#9781);
#2952=VERTEX_POINT('',#9783);
#2953=VERTEX_POINT('',#9787);
#2954=VERTEX_POINT('',#9789);
#2955=VERTEX_POINT('',#9793);
#2956=VERTEX_POINT('',#9794);
#2957=VERTEX_POINT('',#9796);
#2958=VERTEX_POINT('',#9798);
#2959=VERTEX_POINT('',#9802);
#2960=VERTEX_POINT('',#9803);
#2961=VERTEX_POINT('',#9805);
#2962=VERTEX_POINT('',#9807);
#2963=VERTEX_POINT('',#9811);
#2964=VERTEX_POINT('',#9813);
#2965=VERTEX_POINT('',#9817);
#2966=VERTEX_POINT('',#9819);
#2967=VERTEX_POINT('',#9823);
#2968=VERTEX_POINT('',#9825);
#2969=VERTEX_POINT('',#9830);
#2970=VERTEX_POINT('',#9834);
#2971=VERTEX_POINT('',#9844);
#2972=VERTEX_POINT('',#9846);
#2973=VERTEX_POINT('',#9850);
#2974=VERTEX_POINT('',#9852);
#2975=VERTEX_POINT('',#9856);
#2976=VERTEX_POINT('',#9858);
#2977=VERTEX_POINT('',#9862);
#2978=VERTEX_POINT('',#9864);
#2979=VERTEX_POINT('',#9868);
#2980=VERTEX_POINT('',#9870);
#2981=VERTEX_POINT('',#9874);
#2982=VERTEX_POINT('',#9877);
#2983=VERTEX_POINT('',#9881);
#2984=VERTEX_POINT('',#9883);
#2985=VERTEX_POINT('',#9890);
#2986=VERTEX_POINT('',#9892);
#2987=VERTEX_POINT('',#9896);
#2988=VERTEX_POINT('',#9898);
#2989=VERTEX_POINT('',#9902);
#2990=VERTEX_POINT('',#9904);
#2991=VERTEX_POINT('',#9908);
#2992=VERTEX_POINT('',#9910);
#2993=VERTEX_POINT('',#9914);
#2994=VERTEX_POINT('',#9916);
#2995=VERTEX_POINT('',#9920);
#2996=VERTEX_POINT('',#9923);
#2997=VERTEX_POINT('',#9927);
#2998=VERTEX_POINT('',#9929);
#2999=VERTEX_POINT('',#9936);
#3000=VERTEX_POINT('',#9938);
#3001=VERTEX_POINT('',#9943);
#3002=VERTEX_POINT('',#9945);
#3003=VERTEX_POINT('',#9950);
#3004=VERTEX_POINT('',#9952);
#3005=VERTEX_POINT('',#9957);
#3006=VERTEX_POINT('',#9959);
#3007=VERTEX_POINT('',#9964);
#3008=VERTEX_POINT('',#9966);
#3009=VERTEX_POINT('',#9970);
#3010=VERTEX_POINT('',#9973);
#3011=VERTEX_POINT('',#9977);
#3012=VERTEX_POINT('',#9979);
#3013=VERTEX_POINT('',#9983);
#3014=VERTEX_POINT('',#9986);
#3015=VERTEX_POINT('',#9990);
#3016=VERTEX_POINT('',#9992);
#3017=VERTEX_POINT('',#9996);
#3018=VERTEX_POINT('',#9999);
#3019=VERTEX_POINT('',#10003);
#3020=VERTEX_POINT('',#10004);
#3021=VERTEX_POINT('',#10006);
#3022=VERTEX_POINT('',#10008);
#3023=VERTEX_POINT('',#10010);
#3024=VERTEX_POINT('',#10012);
#3025=VERTEX_POINT('',#10014);
#3026=VERTEX_POINT('',#10016);
#3027=VERTEX_POINT('',#10018);
#3028=VERTEX_POINT('',#10020);
#3029=VERTEX_POINT('',#10022);
#3030=VERTEX_POINT('',#10024);
#3031=VERTEX_POINT('',#10028);
#3032=VERTEX_POINT('',#10029);
#3033=VERTEX_POINT('',#10034);
#3034=VERTEX_POINT('',#10035);
#3035=VERTEX_POINT('',#10040);
#3036=VERTEX_POINT('',#10042);
#3037=VERTEX_POINT('',#10046);
#3038=VERTEX_POINT('',#10050);
#3039=VERTEX_POINT('',#10058);
#3040=VERTEX_POINT('',#10060);
#3041=VERTEX_POINT('',#10064);
#3042=VERTEX_POINT('',#10068);
#3043=VERTEX_POINT('',#10078);
#3044=VERTEX_POINT('',#10080);
#3045=VERTEX_POINT('',#10084);
#3046=VERTEX_POINT('',#10086);
#3047=VERTEX_POINT('',#10090);
#3048=VERTEX_POINT('',#10092);
#3049=VERTEX_POINT('',#10096);
#3050=VERTEX_POINT('',#10098);
#3051=VERTEX_POINT('',#10102);
#3052=VERTEX_POINT('',#10104);
#3053=VERTEX_POINT('',#10108);
#3054=VERTEX_POINT('',#10111);
#3055=VERTEX_POINT('',#10115);
#3056=VERTEX_POINT('',#10117);
#3057=VERTEX_POINT('',#11363);
#3058=VERTEX_POINT('',#11365);
#3059=VERTEX_POINT('',#11496);
#3060=VERTEX_POINT('',#11497);
#3061=VERTEX_POINT('',#11500);
#3062=VERTEX_POINT('',#11502);
#3063=VERTEX_POINT('',#11506);
#3064=VERTEX_POINT('',#11510);
#3065=VERTEX_POINT('',#11512);
#3066=VERTEX_POINT('',#11516);
#3067=VERTEX_POINT('',#11521);
#3068=VERTEX_POINT('',#11525);
#3069=VERTEX_POINT('',#11531);
#3070=VERTEX_POINT('',#11532);
#3071=VERTEX_POINT('',#11535);
#3072=VERTEX_POINT('',#11537);
#3073=VERTEX_POINT('',#11541);
#3074=VERTEX_POINT('',#11545);
#3075=VERTEX_POINT('',#11547);
#3076=VERTEX_POINT('',#11550);
#3077=VERTEX_POINT('',#11554);
#3078=VERTEX_POINT('',#11558);
#3079=VERTEX_POINT('',#11566);
#3080=VERTEX_POINT('',#11567);
#3081=VERTEX_POINT('',#11570);
#3082=VERTEX_POINT('',#11571);
#3083=VERTEX_POINT('',#11574);
#3084=VERTEX_POINT('',#11575);
#3085=VERTEX_POINT('',#11578);
#3086=VERTEX_POINT('',#11579);
#3087=VERTEX_POINT('',#11582);
#3088=VERTEX_POINT('',#11583);
#3089=VERTEX_POINT('',#11586);
#3090=VERTEX_POINT('',#11587);
#3091=VERTEX_POINT('',#11590);
#3092=VERTEX_POINT('',#11591);
#3093=VERTEX_POINT('',#11595);
#3094=VERTEX_POINT('',#11596);
#3095=VERTEX_POINT('',#11619);
#3096=VERTEX_POINT('',#11621);
#3097=VERTEX_POINT('',#11646);
#3098=VERTEX_POINT('',#11648);
#3099=VERTEX_POINT('',#11671);
#3100=VERTEX_POINT('',#11673);
#3101=VERTEX_POINT('',#11696);
#3102=VERTEX_POINT('',#11698);
#3103=VERTEX_POINT('',#11701);
#3104=VERTEX_POINT('',#11703);
#3105=VERTEX_POINT('',#11726);
#3106=VERTEX_POINT('',#11728);
#3107=VERTEX_POINT('',#11751);
#3108=VERTEX_POINT('',#11753);
#3109=VERTEX_POINT('',#11776);
#3110=VERTEX_POINT('',#11778);
#3111=VERTEX_POINT('',#11803);
#3112=VERTEX_POINT('',#11807);
#3113=VERTEX_POINT('',#11832);
#3114=VERTEX_POINT('',#11836);
#3115=VERTEX_POINT('',#11861);
#3116=VERTEX_POINT('',#11863);
#3117=VERTEX_POINT('',#11867);
#3118=VERTEX_POINT('',#11892);
#3119=VERTEX_POINT('',#11896);
#3120=VERTEX_POINT('',#11921);
#3121=VERTEX_POINT('',#11925);
#3122=VERTEX_POINT('',#11950);
#3123=VERTEX_POINT('',#11953);
#3124=VERTEX_POINT('',#11955);
#3125=VERTEX_POINT('',#11987);
#3126=VERTEX_POINT('',#11989);
#3127=VERTEX_POINT('',#11992);
#3128=VERTEX_POINT('',#11996);
#3129=VERTEX_POINT('',#12001);
#3130=VERTEX_POINT('',#12003);
#3131=VERTEX_POINT('',#12006);
#3132=VERTEX_POINT('',#12010);
#3133=VERTEX_POINT('',#12021);
#3134=VERTEX_POINT('',#12024);
#3135=VERTEX_POINT('',#12028);
#3136=VERTEX_POINT('',#12032);
#3137=VERTEX_POINT('',#12036);
#3138=VERTEX_POINT('',#12039);
#3139=VERTEX_POINT('',#12043);
#3140=VERTEX_POINT('',#12047);
#3141=VERTEX_POINT('',#12052);
#3142=VERTEX_POINT('',#12053);
#3143=VERTEX_POINT('',#12055);
#3144=VERTEX_POINT('',#12057);
#3145=VERTEX_POINT('',#12061);
#3146=VERTEX_POINT('',#12063);
#3147=VERTEX_POINT('',#12067);
#3148=VERTEX_POINT('',#12069);
#3149=VERTEX_POINT('',#12073);
#3150=VERTEX_POINT('',#12075);
#3151=VERTEX_POINT('',#12079);
#3152=VERTEX_POINT('',#12081);
#3153=VERTEX_POINT('',#12092);
#3154=VERTEX_POINT('',#12093);
#3155=VERTEX_POINT('',#12095);
#3156=VERTEX_POINT('',#12097);
#3157=VERTEX_POINT('',#12101);
#3158=VERTEX_POINT('',#12103);
#3159=VERTEX_POINT('',#12107);
#3160=VERTEX_POINT('',#12109);
#3161=VERTEX_POINT('',#12117);
#3162=VERTEX_POINT('',#12119);
#3163=VERTEX_POINT('',#12122);
#3164=VERTEX_POINT('',#12126);
#3165=VERTEX_POINT('',#12129);
#3166=VERTEX_POINT('',#12133);
#3167=VERTEX_POINT('',#12136);
#3168=VERTEX_POINT('',#12140);
#3169=VERTEX_POINT('',#12143);
#3170=VERTEX_POINT('',#12147);
#3171=VERTEX_POINT('',#12150);
#3172=VERTEX_POINT('',#12154);
#3173=VERTEX_POINT('',#12160);
#3174=VERTEX_POINT('',#12161);
#3175=VERTEX_POINT('',#12163);
#3176=VERTEX_POINT('',#12165);
#3177=VERTEX_POINT('',#12169);
#3178=VERTEX_POINT('',#12171);
#3179=VERTEX_POINT('',#12175);
#3180=VERTEX_POINT('',#12177);
#3181=VERTEX_POINT('',#12184);
#3182=VERTEX_POINT('',#12186);
#3183=VERTEX_POINT('',#12189);
#3184=VERTEX_POINT('',#12193);
#3185=VERTEX_POINT('',#12201);
#3186=VERTEX_POINT('',#12202);
#3187=VERTEX_POINT('',#12204);
#3188=VERTEX_POINT('',#12206);
#3189=VERTEX_POINT('',#12210);
#3190=VERTEX_POINT('',#12212);
#3191=VERTEX_POINT('',#12216);
#3192=VERTEX_POINT('',#12218);
#3193=VERTEX_POINT('',#12222);
#3194=VERTEX_POINT('',#12224);
#3195=VERTEX_POINT('',#12228);
#3196=VERTEX_POINT('',#12230);
#3197=VERTEX_POINT('',#12239);
#3198=VERTEX_POINT('',#12242);
#3199=VERTEX_POINT('',#12245);
#3200=VERTEX_POINT('',#12249);
#3201=VERTEX_POINT('',#12253);
#3202=VERTEX_POINT('',#12257);
#3203=VERTEX_POINT('',#12260);
#3204=VERTEX_POINT('',#12268);
#3205=VERTEX_POINT('',#12270);
#3206=VERTEX_POINT('',#12275);
#3207=VERTEX_POINT('',#12277);
#3208=VERTEX_POINT('',#12282);
#3209=VERTEX_POINT('',#12283);
#3210=VERTEX_POINT('',#12285);
#3211=VERTEX_POINT('',#12287);
#3212=VERTEX_POINT('',#12291);
#3213=VERTEX_POINT('',#12293);
#3214=VERTEX_POINT('',#12297);
#3215=VERTEX_POINT('',#12299);
#3216=VERTEX_POINT('',#12307);
#3217=VERTEX_POINT('',#12308);
#3218=VERTEX_POINT('',#12310);
#3219=VERTEX_POINT('',#12312);
#3220=VERTEX_POINT('',#12316);
#3221=VERTEX_POINT('',#12318);
#3222=VERTEX_POINT('',#12322);
#3223=VERTEX_POINT('',#12324);
#3224=VERTEX_POINT('',#12332);
#3225=VERTEX_POINT('',#12334);
#3226=VERTEX_POINT('',#12341);
#3227=VERTEX_POINT('',#12343);
#3228=VERTEX_POINT('',#12347);
#3229=VERTEX_POINT('',#12349);
#3230=VERTEX_POINT('',#12356);
#3231=VERTEX_POINT('',#12358);
#3232=VERTEX_POINT('',#12362);
#3233=VERTEX_POINT('',#12364);
#3234=VERTEX_POINT('',#12371);
#3235=VERTEX_POINT('',#12373);
#3236=VERTEX_POINT('',#12377);
#3237=VERTEX_POINT('',#12379);
#3238=VERTEX_POINT('',#12386);
#3239=VERTEX_POINT('',#12388);
#3240=VERTEX_POINT('',#12392);
#3241=VERTEX_POINT('',#12394);
#3242=VERTEX_POINT('',#12401);
#3243=VERTEX_POINT('',#12402);
#3244=VERTEX_POINT('',#12404);
#3245=VERTEX_POINT('',#12406);
#3246=VERTEX_POINT('',#12410);
#3247=VERTEX_POINT('',#12412);
#3248=VERTEX_POINT('',#12416);
#3249=VERTEX_POINT('',#12418);
#3250=VERTEX_POINT('',#12422);
#3251=VERTEX_POINT('',#12428);
#3252=VERTEX_POINT('',#12430);
#3253=VERTEX_POINT('',#12434);
#3254=VERTEX_POINT('',#12439);
#3255=VERTEX_POINT('',#12441);
#3256=VERTEX_POINT('',#12448);
#3257=VERTEX_POINT('',#12450);
#3258=VERTEX_POINT('',#12454);
#3259=VERTEX_POINT('',#12455);
#3260=VERTEX_POINT('',#12457);
#3261=VERTEX_POINT('',#12459);
#3262=VERTEX_POINT('',#12463);
#3263=VERTEX_POINT('',#12465);
#3264=VERTEX_POINT('',#12469);
#3265=VERTEX_POINT('',#12471);
#3266=VERTEX_POINT('',#12475);
#3267=VERTEX_POINT('',#12481);
#3268=VERTEX_POINT('',#12482);
#3269=VERTEX_POINT('',#12484);
#3270=VERTEX_POINT('',#12486);
#3271=VERTEX_POINT('',#12490);
#3272=VERTEX_POINT('',#12492);
#3273=VERTEX_POINT('',#12496);
#3274=VERTEX_POINT('',#12500);
#3275=VERTEX_POINT('',#12506);
#3276=VERTEX_POINT('',#12512);
#3277=VERTEX_POINT('',#12514);
#3278=VERTEX_POINT('',#12519);
#3279=VERTEX_POINT('',#12521);
#3280=VERTEX_POINT('',#12528);
#3281=VERTEX_POINT('',#12530);
#3282=VERTEX_POINT('',#12534);
#3283=VERTEX_POINT('',#12536);
#3284=VERTEX_POINT('',#12543);
#3285=VERTEX_POINT('',#12545);
#3286=VERTEX_POINT('',#12549);
#3287=VERTEX_POINT('',#12551);
#3288=VERTEX_POINT('',#12558);
#3289=VERTEX_POINT('',#12559);
#3290=VERTEX_POINT('',#12561);
#3291=VERTEX_POINT('',#12563);
#3292=VERTEX_POINT('',#12565);
#3293=VERTEX_POINT('',#12567);
#3294=VERTEX_POINT('',#12569);
#3295=VERTEX_POINT('',#12571);
#3296=VERTEX_POINT('',#12575);
#3297=VERTEX_POINT('',#12577);
#3298=VERTEX_POINT('',#12581);
#3299=VERTEX_POINT('',#12585);
#3300=VERTEX_POINT('',#12589);
#3301=VERTEX_POINT('',#12593);
#3302=VERTEX_POINT('',#12595);
#3303=VERTEX_POINT('',#12597);
#3304=VERTEX_POINT('',#12609);
#3305=VERTEX_POINT('',#12612);
#3306=VERTEX_POINT('',#12616);
#3307=VERTEX_POINT('',#12620);
#3308=VERTEX_POINT('',#12624);
#3309=VERTEX_POINT('',#12627);
#3310=VERTEX_POINT('',#12631);
#3311=VERTEX_POINT('',#12635);
#3312=VERTEX_POINT('',#12640);
#3313=VERTEX_POINT('',#12641);
#3314=VERTEX_POINT('',#12643);
#3315=VERTEX_POINT('',#12645);
#3316=VERTEX_POINT('',#12649);
#3317=VERTEX_POINT('',#12651);
#3318=VERTEX_POINT('',#12655);
#3319=VERTEX_POINT('',#12657);
#3320=VERTEX_POINT('',#12661);
#3321=VERTEX_POINT('',#12663);
#3322=VERTEX_POINT('',#12667);
#3323=VERTEX_POINT('',#12669);
#3324=VERTEX_POINT('',#12736);
#3325=VERTEX_POINT('',#12738);
#3326=VERTEX_POINT('',#12742);
#3327=VERTEX_POINT('',#12743);
#3328=VERTEX_POINT('',#12745);
#3329=VERTEX_POINT('',#12747);
#3330=VERTEX_POINT('',#12751);
#3331=VERTEX_POINT('',#12753);
#3332=VERTEX_POINT('',#12757);
#3333=VERTEX_POINT('',#12759);
#3334=VERTEX_POINT('',#12769);
#3335=VERTEX_POINT('',#12771);
#3336=VERTEX_POINT('',#12774);
#3337=VERTEX_POINT('',#12779);
#3338=VERTEX_POINT('',#12781);
#3339=VERTEX_POINT('',#12786);
#3340=VERTEX_POINT('',#12792);
#3341=VERTEX_POINT('',#12794);
#3342=VERTEX_POINT('',#12798);
#3343=VERTEX_POINT('',#12800);
#3344=EDGE_CURVE('',#2839,#2840,#1995,.T.);
#3345=EDGE_CURVE('',#2841,#2839,#1996,.T.);
#3346=EDGE_CURVE('',#2842,#2841,#1997,.T.);
#3347=EDGE_CURVE('',#2842,#2840,#1998,.T.);
#3348=EDGE_CURVE('',#2840,#2843,#1999,.T.);
#3349=EDGE_CURVE('',#2844,#2842,#2000,.T.);
#3350=EDGE_CURVE('',#2844,#2843,#2001,.T.);
#3351=EDGE_CURVE('',#2843,#2845,#2002,.T.);
#3352=EDGE_CURVE('',#2846,#2844,#2003,.T.);
#3353=EDGE_CURVE('',#2846,#2845,#2004,.T.);
#3354=EDGE_CURVE('',#2845,#2839,#2005,.T.);
#3355=EDGE_CURVE('',#2841,#2846,#2006,.T.);
#3356=EDGE_CURVE('',#2847,#2847,#659,.T.);
#3357=EDGE_CURVE('',#2847,#2848,#2007,.T.);
#3358=EDGE_CURVE('',#2848,#2848,#660,.T.);
#3359=EDGE_CURVE('',#2849,#2849,#661,.T.);
#3360=EDGE_CURVE('',#2849,#2850,#2008,.T.);
#3361=EDGE_CURVE('',#2850,#2850,#662,.T.);
#3362=EDGE_CURVE('',#2851,#2851,#663,.T.);
#3363=EDGE_CURVE('',#2851,#2852,#2009,.T.);
#3364=EDGE_CURVE('',#2852,#2852,#664,.T.);
#3365=EDGE_CURVE('',#2853,#2853,#665,.T.);
#3366=EDGE_CURVE('',#2853,#2854,#2010,.T.);
#3367=EDGE_CURVE('',#2854,#2854,#666,.T.);
#3368=EDGE_CURVE('',#2855,#2855,#667,.T.);
#3369=EDGE_CURVE('',#2855,#2856,#2011,.T.);
#3370=EDGE_CURVE('',#2856,#2856,#668,.T.);
#3371=EDGE_CURVE('',#2857,#2857,#669,.T.);
#3372=EDGE_CURVE('',#2857,#2858,#2012,.T.);
#3373=EDGE_CURVE('',#2858,#2858,#670,.T.);
#3374=EDGE_CURVE('',#2859,#2860,#2013,.T.);
#3375=EDGE_CURVE('',#2860,#2861,#2014,.T.);
#3376=EDGE_CURVE('',#2862,#2861,#2015,.T.);
#3377=EDGE_CURVE('',#2859,#2862,#2016,.T.);
#3378=EDGE_CURVE('',#2863,#2859,#2017,.T.);
#3379=EDGE_CURVE('',#2864,#2862,#2018,.T.);
#3380=EDGE_CURVE('',#2863,#2864,#2019,.T.);
#3381=EDGE_CURVE('',#2865,#2863,#2020,.T.);
#3382=EDGE_CURVE('',#2866,#2864,#2021,.T.);
#3383=EDGE_CURVE('',#2865,#2866,#2022,.T.);
#3384=EDGE_CURVE('',#2860,#2865,#2023,.T.);
#3385=EDGE_CURVE('',#2861,#2866,#2024,.T.);
#3386=EDGE_CURVE('',#2867,#2868,#2025,.T.);
#3387=EDGE_CURVE('',#2868,#2869,#2026,.T.);
#3388=EDGE_CURVE('',#2870,#2869,#2027,.T.);
#3389=EDGE_CURVE('',#2867,#2870,#2028,.T.);
#3390=EDGE_CURVE('',#2871,#2867,#2029,.T.);
#3391=EDGE_CURVE('',#2872,#2870,#2030,.T.);
#3392=EDGE_CURVE('',#2871,#2872,#2031,.T.);
#3393=EDGE_CURVE('',#2873,#2871,#2032,.T.);
#3394=EDGE_CURVE('',#2874,#2872,#2033,.T.);
#3395=EDGE_CURVE('',#2873,#2874,#2034,.T.);
#3396=EDGE_CURVE('',#2868,#2873,#2035,.T.);
#3397=EDGE_CURVE('',#2869,#2874,#2036,.T.);
#3398=EDGE_CURVE('',#2875,#2876,#2037,.T.);
#3399=EDGE_CURVE('',#2876,#2877,#2038,.T.);
#3400=EDGE_CURVE('',#2878,#2877,#2039,.T.);
#3401=EDGE_CURVE('',#2875,#2878,#2040,.T.);
#3402=EDGE_CURVE('',#2879,#2875,#2041,.T.);
#3403=EDGE_CURVE('',#2880,#2878,#2042,.T.);
#3404=EDGE_CURVE('',#2879,#2880,#2043,.T.);
#3405=EDGE_CURVE('',#2881,#2879,#2044,.T.);
#3406=EDGE_CURVE('',#2882,#2880,#2045,.T.);
#3407=EDGE_CURVE('',#2881,#2882,#2046,.T.);
#3408=EDGE_CURVE('',#2876,#2881,#2047,.T.);
#3409=EDGE_CURVE('',#2877,#2882,#2048,.T.);
#3410=EDGE_CURVE('',#2883,#2883,#671,.T.);
#3411=EDGE_CURVE('',#2883,#2884,#2049,.T.);
#3412=EDGE_CURVE('',#2884,#2884,#672,.T.);
#3413=EDGE_CURVE('',#2885,#2885,#673,.T.);
#3414=EDGE_CURVE('',#2885,#2886,#2050,.T.);
#3415=EDGE_CURVE('',#2886,#2886,#674,.T.);
#3416=EDGE_CURVE('',#2887,#2887,#675,.T.);
#3417=EDGE_CURVE('',#2887,#2888,#2051,.T.);
#3418=EDGE_CURVE('',#2888,#2888,#676,.T.);
#3419=EDGE_CURVE('',#2889,#2889,#677,.T.);
#3420=EDGE_CURVE('',#2889,#2890,#2052,.T.);
#3421=EDGE_CURVE('',#2890,#2890,#678,.T.);
#3422=EDGE_CURVE('',#2891,#2891,#679,.T.);
#3423=EDGE_CURVE('',#2891,#2892,#2053,.T.);
#3424=EDGE_CURVE('',#2892,#2892,#680,.T.);
#3425=EDGE_CURVE('',#2893,#2893,#681,.T.);
#3426=EDGE_CURVE('',#2893,#2894,#2054,.T.);
#3427=EDGE_CURVE('',#2894,#2894,#682,.T.);
#3428=EDGE_CURVE('',#2895,#2895,#683,.T.);
#3429=EDGE_CURVE('',#2895,#2896,#2055,.T.);
#3430=EDGE_CURVE('',#2896,#2896,#684,.T.);
#3431=EDGE_CURVE('',#2897,#2898,#2056,.T.);
#3432=EDGE_CURVE('',#2899,#2897,#2057,.T.);
#3433=EDGE_CURVE('',#2899,#2900,#2058,.T.);
#3434=EDGE_CURVE('',#2898,#2900,#2059,.T.);
#3435=EDGE_CURVE('',#2901,#2902,#2060,.T.);
#3436=EDGE_CURVE('',#2903,#2901,#2061,.T.);
#3437=EDGE_CURVE('',#2904,#2903,#2062,.T.);
#3438=EDGE_CURVE('',#2902,#2904,#2063,.T.);
#3439=EDGE_CURVE('',#2904,#2905,#2064,.T.);
#3440=EDGE_CURVE('',#2906,#2903,#2065,.T.);
#3441=EDGE_CURVE('',#2905,#2906,#2066,.T.);
#3442=EDGE_CURVE('',#2907,#2899,#2067,.T.);
#3443=EDGE_CURVE('',#2907,#2908,#2068,.T.);
#3444=EDGE_CURVE('',#2900,#2908,#2069,.T.);
#3445=EDGE_CURVE('',#2897,#2909,#2070,.T.);
#3446=EDGE_CURVE('',#2910,#2909,#2071,.T.);
#3447=EDGE_CURVE('',#2902,#2910,#2072,.T.);
#3448=EDGE_CURVE('',#2905,#2907,#2073,.T.);
#3449=EDGE_CURVE('',#2898,#2911,#2074,.T.);
#3450=EDGE_CURVE('',#2909,#2911,#2075,.T.);
#3451=EDGE_CURVE('',#2901,#2912,#2076,.T.);
#3452=EDGE_CURVE('',#2911,#2912,#2077,.T.);
#3453=EDGE_CURVE('',#2908,#2906,#2078,.T.);
#3454=EDGE_CURVE('',#2912,#2910,#2079,.T.);
#3455=EDGE_CURVE('',#2913,#2913,#685,.T.);
#3456=EDGE_CURVE('',#2913,#2914,#2080,.T.);
#3457=EDGE_CURVE('',#2914,#2914,#686,.T.);
#3458=EDGE_CURVE('',#2915,#2915,#687,.T.);
#3459=EDGE_CURVE('',#2915,#2916,#2081,.T.);
#3460=EDGE_CURVE('',#2916,#2916,#688,.T.);
#3461=EDGE_CURVE('',#2917,#2917,#689,.T.);
#3462=EDGE_CURVE('',#2917,#2918,#2082,.T.);
#3463=EDGE_CURVE('',#2918,#2918,#690,.T.);
#3464=EDGE_CURVE('',#2919,#2919,#691,.T.);
#3465=EDGE_CURVE('',#2919,#2920,#2083,.T.);
#3466=EDGE_CURVE('',#2920,#2920,#692,.T.);
#3467=EDGE_CURVE('',#2921,#2921,#693,.T.);
#3468=EDGE_CURVE('',#2921,#2922,#2084,.T.);
#3469=EDGE_CURVE('',#2922,#2922,#694,.T.);
#3470=EDGE_CURVE('',#2923,#2923,#695,.T.);
#3471=EDGE_CURVE('',#2923,#2924,#2085,.T.);
#3472=EDGE_CURVE('',#2924,#2924,#696,.T.);
#3473=EDGE_CURVE('',#2925,#2925,#697,.T.);
#3474=EDGE_CURVE('',#2925,#2926,#2086,.T.);
#3475=EDGE_CURVE('',#2926,#2926,#698,.T.);
#3476=EDGE_CURVE('',#2927,#2927,#699,.T.);
#3477=EDGE_CURVE('',#2927,#2928,#2087,.T.);
#3478=EDGE_CURVE('',#2928,#2928,#700,.T.);
#3479=EDGE_CURVE('',#2929,#2929,#701,.T.);
#3480=EDGE_CURVE('',#2929,#2930,#2088,.T.);
#3481=EDGE_CURVE('',#2930,#2930,#702,.T.);
#3482=EDGE_CURVE('',#2931,#2931,#703,.T.);
#3483=EDGE_CURVE('',#2931,#2932,#2089,.T.);
#3484=EDGE_CURVE('',#2932,#2932,#704,.T.);
#3485=EDGE_CURVE('',#2933,#2933,#705,.T.);
#3486=EDGE_CURVE('',#2933,#2934,#2090,.T.);
#3487=EDGE_CURVE('',#2934,#2934,#706,.T.);
#3488=EDGE_CURVE('',#2935,#2935,#707,.T.);
#3489=EDGE_CURVE('',#2935,#2936,#2091,.T.);
#3490=EDGE_CURVE('',#2936,#2936,#708,.T.);
#3491=EDGE_CURVE('',#2937,#2937,#709,.T.);
#3492=EDGE_CURVE('',#2938,#2938,#710,.T.);
#3493=EDGE_CURVE('',#2938,#2937,#2092,.T.);
#3494=EDGE_CURVE('',#2939,#2939,#711,.T.);
#3495=EDGE_CURVE('',#2939,#2940,#2093,.T.);
#3496=EDGE_CURVE('',#2940,#2940,#712,.T.);
#3497=EDGE_CURVE('',#2941,#2941,#713,.T.);
#3498=EDGE_CURVE('',#2941,#2942,#2094,.T.);
#3499=EDGE_CURVE('',#2942,#2942,#714,.T.);
#3500=EDGE_CURVE('',#2943,#2943,#715,.T.);
#3501=EDGE_CURVE('',#2943,#2944,#2095,.T.);
#3502=EDGE_CURVE('',#2944,#2944,#716,.T.);
#3503=EDGE_CURVE('',#2945,#2945,#717,.T.);
#3504=EDGE_CURVE('',#2945,#2946,#2096,.T.);
#3505=EDGE_CURVE('',#2946,#2946,#718,.T.);
#3506=EDGE_CURVE('',#2947,#2947,#719,.T.);
#3507=EDGE_CURVE('',#2947,#2948,#2097,.T.);
#3508=EDGE_CURVE('',#2948,#2948,#720,.T.);
#3509=EDGE_CURVE('',#2949,#2949,#721,.T.);
#3510=EDGE_CURVE('',#2949,#2950,#2098,.T.);
#3511=EDGE_CURVE('',#2950,#2950,#722,.T.);
#3512=EDGE_CURVE('',#2951,#2951,#723,.T.);
#3513=EDGE_CURVE('',#2951,#2952,#2099,.T.);
#3514=EDGE_CURVE('',#2952,#2952,#724,.T.);
#3515=EDGE_CURVE('',#2953,#2953,#725,.T.);
#3516=EDGE_CURVE('',#2953,#2954,#2100,.T.);
#3517=EDGE_CURVE('',#2954,#2954,#726,.T.);
#3518=EDGE_CURVE('',#2955,#2956,#2101,.T.);
#3519=EDGE_CURVE('',#2957,#2955,#2102,.T.);
#3520=EDGE_CURVE('',#2957,#2958,#2103,.T.);
#3521=EDGE_CURVE('',#2956,#2958,#2104,.T.);
#3522=EDGE_CURVE('',#2959,#2960,#2105,.T.);
#3523=EDGE_CURVE('',#2961,#2959,#2106,.T.);
#3524=EDGE_CURVE('',#2962,#2961,#2107,.T.);
#3525=EDGE_CURVE('',#2960,#2962,#2108,.T.);
#3526=EDGE_CURVE('',#2962,#2963,#2109,.T.);
#3527=EDGE_CURVE('',#2964,#2961,#2110,.T.);
#3528=EDGE_CURVE('',#2963,#2964,#2111,.T.);
#3529=EDGE_CURVE('',#2965,#2957,#2112,.T.);
#3530=EDGE_CURVE('',#2965,#2966,#2113,.T.);
#3531=EDGE_CURVE('',#2958,#2966,#2114,.T.);
#3532=EDGE_CURVE('',#2955,#2967,#2115,.T.);
#3533=EDGE_CURVE('',#2968,#2967,#2116,.T.);
#3534=EDGE_CURVE('',#2960,#2968,#2117,.T.);
#3535=EDGE_CURVE('',#2963,#2965,#2118,.T.);
#3536=EDGE_CURVE('',#2956,#2969,#2119,.T.);
#3537=EDGE_CURVE('',#2967,#2969,#2120,.T.);
#3538=EDGE_CURVE('',#2959,#2970,#2121,.T.);
#3539=EDGE_CURVE('',#2969,#2970,#2122,.T.);
#3540=EDGE_CURVE('',#2966,#2964,#2123,.T.);
#3541=EDGE_CURVE('',#2970,#2968,#2124,.T.);
#3542=EDGE_CURVE('',#2971,#2971,#727,.T.);
#3543=EDGE_CURVE('',#2971,#2972,#2125,.T.);
#3544=EDGE_CURVE('',#2972,#2972,#728,.T.);
#3545=EDGE_CURVE('',#2973,#2973,#729,.T.);
#3546=EDGE_CURVE('',#2973,#2974,#2126,.T.);
#3547=EDGE_CURVE('',#2974,#2974,#730,.T.);
#3548=EDGE_CURVE('',#2975,#2975,#731,.T.);
#3549=EDGE_CURVE('',#2975,#2976,#2127,.T.);
#3550=EDGE_CURVE('',#2976,#2976,#732,.T.);
#3551=EDGE_CURVE('',#2977,#2977,#733,.T.);
#3552=EDGE_CURVE('',#2977,#2978,#2128,.T.);
#3553=EDGE_CURVE('',#2978,#2978,#734,.T.);
#3554=EDGE_CURVE('',#2979,#2979,#735,.T.);
#3555=EDGE_CURVE('',#2979,#2980,#2129,.T.);
#3556=EDGE_CURVE('',#2980,#2980,#736,.T.);
#3557=EDGE_CURVE('',#2981,#2981,#737,.T.);
#3558=EDGE_CURVE('',#2981,#2982,#2130,.T.);
#3559=EDGE_CURVE('',#2982,#2982,#738,.T.);
#3560=EDGE_CURVE('',#2983,#2983,#739,.T.);
#3561=EDGE_CURVE('',#2983,#2984,#2131,.T.);
#3562=EDGE_CURVE('',#2984,#2984,#740,.T.);
#3563=EDGE_CURVE('',#2985,#2985,#741,.T.);
#3564=EDGE_CURVE('',#2985,#2986,#2132,.T.);
#3565=EDGE_CURVE('',#2986,#2986,#742,.T.);
#3566=EDGE_CURVE('',#2987,#2987,#743,.T.);
#3567=EDGE_CURVE('',#2987,#2988,#2133,.T.);
#3568=EDGE_CURVE('',#2988,#2988,#744,.T.);
#3569=EDGE_CURVE('',#2989,#2989,#745,.T.);
#3570=EDGE_CURVE('',#2989,#2990,#2134,.T.);
#3571=EDGE_CURVE('',#2990,#2990,#746,.T.);
#3572=EDGE_CURVE('',#2991,#2991,#747,.T.);
#3573=EDGE_CURVE('',#2991,#2992,#2135,.T.);
#3574=EDGE_CURVE('',#2992,#2992,#748,.T.);
#3575=EDGE_CURVE('',#2993,#2993,#749,.T.);
#3576=EDGE_CURVE('',#2993,#2994,#2136,.T.);
#3577=EDGE_CURVE('',#2994,#2994,#750,.T.);
#3578=EDGE_CURVE('',#2995,#2995,#751,.T.);
#3579=EDGE_CURVE('',#2996,#2996,#752,.T.);
#3580=EDGE_CURVE('',#2996,#2995,#2137,.T.);
#3581=EDGE_CURVE('',#2997,#2997,#753,.T.);
#3582=EDGE_CURVE('',#2997,#2998,#2138,.T.);
#3583=EDGE_CURVE('',#2998,#2998,#754,.T.);
#3584=EDGE_CURVE('',#2999,#2999,#755,.T.);
#3585=EDGE_CURVE('',#2999,#3000,#2139,.T.);
#3586=EDGE_CURVE('',#3000,#3000,#756,.T.);
#3587=EDGE_CURVE('',#3001,#3001,#757,.T.);
#3588=EDGE_CURVE('',#3001,#3002,#2140,.T.);
#3589=EDGE_CURVE('',#3002,#3002,#758,.T.);
#3590=EDGE_CURVE('',#3003,#3003,#759,.T.);
#3591=EDGE_CURVE('',#3003,#3004,#2141,.T.);
#3592=EDGE_CURVE('',#3004,#3004,#760,.T.);
#3593=EDGE_CURVE('',#3005,#3005,#761,.T.);
#3594=EDGE_CURVE('',#3005,#3006,#2142,.T.);
#3595=EDGE_CURVE('',#3006,#3006,#762,.T.);
#3596=EDGE_CURVE('',#3007,#3007,#763,.T.);
#3597=EDGE_CURVE('',#3007,#3008,#2143,.T.);
#3598=EDGE_CURVE('',#3008,#3008,#764,.T.);
#3599=EDGE_CURVE('',#3009,#3009,#765,.T.);
#3600=EDGE_CURVE('',#3010,#3010,#766,.T.);
#3601=EDGE_CURVE('',#3010,#3009,#2144,.T.);
#3602=EDGE_CURVE('',#3011,#3011,#767,.T.);
#3603=EDGE_CURVE('',#3011,#3012,#2145,.T.);
#3604=EDGE_CURVE('',#3012,#3012,#768,.T.);
#3605=EDGE_CURVE('',#3013,#3013,#769,.T.);
#3606=EDGE_CURVE('',#3014,#3014,#770,.T.);
#3607=EDGE_CURVE('',#3014,#3013,#2146,.T.);
#3608=EDGE_CURVE('',#3015,#3015,#771,.T.);
#3609=EDGE_CURVE('',#3015,#3016,#2147,.T.);
#3610=EDGE_CURVE('',#3016,#3016,#772,.T.);
#3611=EDGE_CURVE('',#3017,#3017,#773,.T.);
#3612=EDGE_CURVE('',#3018,#3018,#774,.T.);
#3613=EDGE_CURVE('',#3018,#3017,#2148,.T.);
#3614=EDGE_CURVE('',#3019,#3020,#2149,.T.);
#3615=EDGE_CURVE('',#3019,#3021,#2150,.T.);
#3616=EDGE_CURVE('',#3022,#3021,#2151,.T.);
#3617=EDGE_CURVE('',#3023,#3022,#2152,.T.);
#3618=EDGE_CURVE('',#3024,#3023,#2153,.T.);
#3619=EDGE_CURVE('',#3025,#3024,#2154,.T.);
#3620=EDGE_CURVE('',#3026,#3025,#2155,.T.);
#3621=EDGE_CURVE('',#3027,#3026,#2156,.T.);
#3622=EDGE_CURVE('',#3028,#3027,#2157,.T.);
#3623=EDGE_CURVE('',#3028,#3029,#2158,.T.);
#3624=EDGE_CURVE('',#3030,#3029,#2159,.T.);
#3625=EDGE_CURVE('',#3020,#3030,#2160,.T.);
#3626=EDGE_CURVE('',#3031,#3032,#2161,.T.);
#3627=EDGE_CURVE('',#3032,#3022,#2162,.T.);
#3628=EDGE_CURVE('',#3021,#3031,#2163,.T.);
#3629=EDGE_CURVE('',#3033,#3034,#2164,.T.);
#3630=EDGE_CURVE('',#3034,#3028,#2165,.T.);
#3631=EDGE_CURVE('',#3027,#3033,#2166,.T.);
#3632=EDGE_CURVE('',#3035,#3024,#2167,.T.);
#3633=EDGE_CURVE('',#3036,#3035,#2168,.T.);
#3634=EDGE_CURVE('',#3025,#3036,#2169,.T.);
#3635=EDGE_CURVE('',#3023,#3037,#2170,.T.);
#3636=EDGE_CURVE('',#3037,#3035,#2171,.T.);
#3637=EDGE_CURVE('',#3036,#3038,#2172,.T.);
#3638=EDGE_CURVE('',#3038,#3037,#2173,.T.);
#3639=EDGE_CURVE('',#3038,#3026,#2174,.T.);
#3640=EDGE_CURVE('',#3033,#3032,#2175,.T.);
#3641=EDGE_CURVE('',#3039,#3030,#2176,.T.);
#3642=EDGE_CURVE('',#3039,#3040,#2177,.T.);
#3643=EDGE_CURVE('',#3040,#3020,#2178,.T.);
#3644=EDGE_CURVE('',#3041,#3029,#2179,.T.);
#3645=EDGE_CURVE('',#3041,#3039,#2180,.T.);
#3646=EDGE_CURVE('',#3040,#3042,#2181,.T.);
#3647=EDGE_CURVE('',#3042,#3019,#2182,.T.);
#3648=EDGE_CURVE('',#3042,#3041,#2183,.T.);
#3649=EDGE_CURVE('',#3034,#3031,#2184,.T.);
#3650=EDGE_CURVE('',#3043,#3043,#775,.T.);
#3651=EDGE_CURVE('',#3043,#3044,#2185,.T.);
#3652=EDGE_CURVE('',#3044,#3044,#776,.T.);
#3653=EDGE_CURVE('',#3045,#3045,#777,.T.);
#3654=EDGE_CURVE('',#3045,#3046,#2186,.T.);
#3655=EDGE_CURVE('',#3046,#3046,#778,.T.);
#3656=EDGE_CURVE('',#3047,#3047,#779,.T.);
#3657=EDGE_CURVE('',#3047,#3048,#2187,.T.);
#3658=EDGE_CURVE('',#3048,#3048,#780,.T.);
#3659=EDGE_CURVE('',#3049,#3049,#781,.T.);
#3660=EDGE_CURVE('',#3049,#3050,#2188,.T.);
#3661=EDGE_CURVE('',#3050,#3050,#782,.T.);
#3662=EDGE_CURVE('',#3051,#3051,#783,.T.);
#3663=EDGE_CURVE('',#3051,#3052,#2189,.T.);
#3664=EDGE_CURVE('',#3052,#3052,#784,.T.);
#3665=EDGE_CURVE('',#3053,#3053,#785,.T.);
#3666=EDGE_CURVE('',#3054,#3054,#786,.T.);
#3667=EDGE_CURVE('',#3054,#3053,#2190,.T.);
#3668=EDGE_CURVE('',#3055,#3055,#787,.T.);
#3669=EDGE_CURVE('',#3055,#3056,#2191,.T.);
#3670=EDGE_CURVE('',#3056,#3056,#788,.T.);
#3671=EDGE_CURVE('',#3057,#3057,#789,.T.);
#3672=EDGE_CURVE('',#3057,#3058,#324,.T.);
#3673=EDGE_CURVE('',#3058,#3058,#790,.T.);
#3674=EDGE_CURVE('',#3059,#3060,#791,.T.);
#3675=EDGE_CURVE('',#3060,#3059,#792,.T.);
#3676=EDGE_CURVE('',#3060,#3061,#793,.T.);
#3677=EDGE_CURVE('',#3062,#3061,#794,.T.);
#3678=EDGE_CURVE('',#3061,#3062,#795,.T.);
#3679=EDGE_CURVE('',#3062,#3063,#2192,.T.);
#3680=EDGE_CURVE('',#3063,#3063,#796,.T.);
#3681=EDGE_CURVE('',#3064,#3064,#797,.T.);
#3682=EDGE_CURVE('',#3064,#3065,#2193,.T.);
#3683=EDGE_CURVE('',#3065,#3065,#798,.T.);
#3684=EDGE_CURVE('',#3065,#3066,#2194,.T.);
#3685=EDGE_CURVE('',#3066,#3066,#799,.T.);
#3686=EDGE_CURVE('',#3067,#3067,#800,.T.);
#3687=EDGE_CURVE('',#3067,#3059,#2195,.T.);
#3688=EDGE_CURVE('',#3068,#3068,#801,.T.);
#3689=EDGE_CURVE('',#3068,#3064,#2196,.T.);
#3690=EDGE_CURVE('',#3069,#3070,#802,.T.);
#3691=EDGE_CURVE('',#3070,#3069,#803,.T.);
#3692=EDGE_CURVE('',#3070,#3071,#804,.T.);
#3693=EDGE_CURVE('',#3072,#3071,#805,.T.);
#3694=EDGE_CURVE('',#3071,#3072,#806,.T.);
#3695=EDGE_CURVE('',#3073,#3073,#807,.T.);
#3696=EDGE_CURVE('',#3073,#3072,#2197,.T.);
#3697=EDGE_CURVE('',#3074,#3074,#808,.T.);
#3698=EDGE_CURVE('',#3075,#3075,#809,.T.);
#3699=EDGE_CURVE('',#3076,#3076,#810,.T.);
#3700=EDGE_CURVE('',#3076,#3074,#2198,.T.);
#3701=EDGE_CURVE('',#3077,#3077,#811,.T.);
#3702=EDGE_CURVE('',#3077,#3076,#2199,.T.);
#3703=EDGE_CURVE('',#3078,#3078,#812,.T.);
#3704=EDGE_CURVE('',#3078,#3077,#2200,.T.);
#3705=EDGE_CURVE('',#3069,#3075,#2201,.T.);
#3706=EDGE_CURVE('',#3079,#3080,#813,.T.);
#3707=EDGE_CURVE('',#3081,#3082,#814,.T.);
#3708=EDGE_CURVE('',#3083,#3084,#815,.T.);
#3709=EDGE_CURVE('',#3085,#3086,#816,.T.);
#3710=EDGE_CURVE('',#3087,#3088,#817,.T.);
#3711=EDGE_CURVE('',#3089,#3090,#818,.T.);
#3712=EDGE_CURVE('',#3091,#3092,#819,.T.);
#3713=EDGE_CURVE('',#3093,#3094,#325,.T.);
#3714=EDGE_CURVE('',#3095,#3093,#820,.T.);
#3715=EDGE_CURVE('',#3096,#3095,#326,.T.);
#3716=EDGE_CURVE('',#3094,#3096,#821,.T.);
#3717=EDGE_CURVE('',#3097,#3095,#822,.T.);
#3718=EDGE_CURVE('',#3097,#3098,#327,.T.);
#3719=EDGE_CURVE('',#3099,#3098,#823,.T.);
#3720=EDGE_CURVE('',#3099,#3100,#328,.T.);
#3721=EDGE_CURVE('',#3101,#3100,#824,.T.);
#3722=EDGE_CURVE('',#3101,#3102,#2202,.T.);
#3723=EDGE_CURVE('',#3102,#3102,#825,.T.);
#3724=EDGE_CURVE('',#3103,#3101,#826,.T.);
#3725=EDGE_CURVE('',#3103,#3104,#329,.T.);
#3726=EDGE_CURVE('',#3105,#3104,#827,.T.);
#3727=EDGE_CURVE('',#3105,#3106,#330,.T.);
#3728=EDGE_CURVE('',#3107,#3106,#828,.T.);
#3729=EDGE_CURVE('',#3107,#3108,#331,.T.);
#3730=EDGE_CURVE('',#3109,#3108,#829,.T.);
#3731=EDGE_CURVE('',#3109,#3110,#332,.T.);
#3732=EDGE_CURVE('',#3096,#3110,#830,.T.);
#3733=EDGE_CURVE('',#3093,#3111,#831,.T.);
#3734=EDGE_CURVE('',#3111,#3097,#832,.T.);
#3735=EDGE_CURVE('',#3112,#3111,#333,.T.);
#3736=EDGE_CURVE('',#3098,#3112,#833,.T.);
#3737=EDGE_CURVE('',#3112,#3113,#834,.T.);
#3738=EDGE_CURVE('',#3113,#3099,#835,.T.);
#3739=EDGE_CURVE('',#3114,#3113,#334,.T.);
#3740=EDGE_CURVE('',#3100,#3114,#836,.T.);
#3741=EDGE_CURVE('',#3114,#3115,#837,.T.);
#3742=EDGE_CURVE('',#3115,#3116,#838,.T.);
#3743=EDGE_CURVE('',#3116,#3103,#839,.T.);
#3744=EDGE_CURVE('',#3117,#3116,#335,.T.);
#3745=EDGE_CURVE('',#3104,#3117,#840,.T.);
#3746=EDGE_CURVE('',#3117,#3118,#841,.T.);
#3747=EDGE_CURVE('',#3118,#3105,#842,.T.);
#3748=EDGE_CURVE('',#3119,#3118,#336,.T.);
#3749=EDGE_CURVE('',#3106,#3119,#843,.T.);
#3750=EDGE_CURVE('',#3119,#3120,#844,.T.);
#3751=EDGE_CURVE('',#3120,#3107,#845,.T.);
#3752=EDGE_CURVE('',#3121,#3120,#337,.T.);
#3753=EDGE_CURVE('',#3108,#3121,#846,.T.);
#3754=EDGE_CURVE('',#3122,#3122,#847,.T.);
#3755=EDGE_CURVE('',#3122,#3115,#2203,.T.);
#3756=EDGE_CURVE('',#3123,#3094,#848,.T.);
#3757=EDGE_CURVE('',#3123,#3124,#338,.T.);
#3758=EDGE_CURVE('',#3121,#3124,#849,.T.);
#3759=EDGE_CURVE('',#3110,#3123,#850,.T.);
#3760=EDGE_CURVE('',#3124,#3109,#851,.T.);
#3761=EDGE_CURVE('',#3125,#3125,#852,.T.);
#3762=EDGE_CURVE('',#3126,#3126,#853,.T.);
#3763=EDGE_CURVE('',#3127,#3127,#854,.T.);
#3764=EDGE_CURVE('',#3127,#3125,#2204,.T.);
#3765=EDGE_CURVE('',#3128,#3128,#855,.T.);
#3766=EDGE_CURVE('',#3128,#3126,#2205,.T.);
#3767=EDGE_CURVE('',#3129,#3129,#856,.T.);
#3768=EDGE_CURVE('',#3130,#3130,#857,.T.);
#3769=EDGE_CURVE('',#3131,#3131,#858,.T.);
#3770=EDGE_CURVE('',#3131,#3129,#2206,.T.);
#3771=EDGE_CURVE('',#3132,#3132,#859,.T.);
#3772=EDGE_CURVE('',#3132,#3130,#2207,.T.);
#3773=EDGE_CURVE('',#3133,#3133,#860,.T.);
#3774=EDGE_CURVE('',#3134,#3134,#861,.T.);
#3775=EDGE_CURVE('',#3134,#3133,#2208,.T.);
#3776=EDGE_CURVE('',#3135,#3135,#862,.T.);
#3777=EDGE_CURVE('',#3135,#3134,#2209,.T.);
#3778=EDGE_CURVE('',#3136,#3136,#863,.T.);
#3779=EDGE_CURVE('',#3136,#3135,#2210,.T.);
#3780=EDGE_CURVE('',#3137,#3137,#864,.T.);
#3781=EDGE_CURVE('',#3138,#3138,#865,.F.);
#3782=EDGE_CURVE('',#3138,#3137,#2211,.T.);
#3783=EDGE_CURVE('',#3139,#3139,#866,.F.);
#3784=EDGE_CURVE('',#3139,#3138,#2212,.T.);
#3785=EDGE_CURVE('',#3140,#3140,#867,.T.);
#3786=EDGE_CURVE('',#3140,#3139,#2213,.T.);
#3787=EDGE_CURVE('',#3141,#3142,#2214,.T.);
#3788=EDGE_CURVE('',#3142,#3143,#2215,.T.);
#3789=EDGE_CURVE('',#3143,#3144,#2216,.T.);
#3790=EDGE_CURVE('',#3141,#3144,#2217,.T.);
#3791=EDGE_CURVE('',#3142,#3145,#2218,.T.);
#3792=EDGE_CURVE('',#3145,#3146,#2219,.T.);
#3793=EDGE_CURVE('',#3146,#3143,#2220,.T.);
#3794=EDGE_CURVE('',#3145,#3147,#2221,.T.);
#3795=EDGE_CURVE('',#3147,#3148,#2222,.T.);
#3796=EDGE_CURVE('',#3148,#3146,#2223,.T.);
#3797=EDGE_CURVE('',#3147,#3149,#2224,.T.);
#3798=EDGE_CURVE('',#3149,#3150,#2225,.T.);
#3799=EDGE_CURVE('',#3150,#3148,#2226,.T.);
#3800=EDGE_CURVE('',#3149,#3151,#2227,.T.);
#3801=EDGE_CURVE('',#3151,#3152,#2228,.T.);
#3802=EDGE_CURVE('',#3152,#3150,#2229,.T.);
#3803=EDGE_CURVE('',#3151,#3141,#2230,.T.);
#3804=EDGE_CURVE('',#3144,#3152,#2231,.T.);
#3805=EDGE_CURVE('',#3153,#3154,#868,.T.);
#3806=EDGE_CURVE('',#3155,#3153,#2232,.T.);
#3807=EDGE_CURVE('',#3156,#3155,#2233,.T.);
#3808=EDGE_CURVE('',#3154,#3156,#2234,.T.);
#3809=EDGE_CURVE('',#3154,#3157,#2235,.T.);
#3810=EDGE_CURVE('',#3158,#3156,#2236,.T.);
#3811=EDGE_CURVE('',#3158,#3157,#2237,.T.);
#3812=EDGE_CURVE('',#3157,#3159,#869,.T.);
#3813=EDGE_CURVE('',#3160,#3158,#2238,.T.);
#3814=EDGE_CURVE('',#3159,#3160,#2239,.T.);
#3815=EDGE_CURVE('',#3159,#3153,#2240,.T.);
#3816=EDGE_CURVE('',#3160,#3155,#2241,.T.);
#3817=EDGE_CURVE('',#3161,#3161,#870,.T.);
#3818=EDGE_CURVE('',#3162,#3162,#871,.T.);
#3819=EDGE_CURVE('',#3163,#3163,#872,.T.);
#3820=EDGE_CURVE('',#3163,#3161,#2242,.T.);
#3821=EDGE_CURVE('',#3164,#3164,#873,.T.);
#3822=EDGE_CURVE('',#3165,#3165,#874,.T.);
#3823=EDGE_CURVE('',#3165,#3164,#2243,.T.);
#3824=EDGE_CURVE('',#3166,#3166,#875,.T.);
#3825=EDGE_CURVE('',#3167,#3167,#876,.T.);
#3826=EDGE_CURVE('',#3167,#3166,#2244,.T.);
#3827=EDGE_CURVE('',#3168,#3168,#877,.T.);
#3828=EDGE_CURVE('',#3169,#3169,#878,.T.);
#3829=EDGE_CURVE('',#3169,#3168,#2245,.T.);
#3830=EDGE_CURVE('',#3170,#3170,#879,.T.);
#3831=EDGE_CURVE('',#3171,#3171,#880,.T.);
#3832=EDGE_CURVE('',#3171,#3170,#2246,.T.);
#3833=EDGE_CURVE('',#3172,#3172,#881,.T.);
#3834=EDGE_CURVE('',#3172,#3162,#2247,.T.);
#3835=EDGE_CURVE('',#3173,#3174,#882,.T.);
#3836=EDGE_CURVE('',#3175,#3173,#2248,.T.);
#3837=EDGE_CURVE('',#3176,#3175,#883,.T.);
#3838=EDGE_CURVE('',#3174,#3176,#2249,.T.);
#3839=EDGE_CURVE('',#3174,#3177,#2250,.T.);
#3840=EDGE_CURVE('',#3178,#3176,#2251,.T.);
#3841=EDGE_CURVE('',#3178,#3177,#2252,.T.);
#3842=EDGE_CURVE('',#3177,#3179,#884,.T.);
#3843=EDGE_CURVE('',#3180,#3178,#885,.T.);
#3844=EDGE_CURVE('',#3179,#3180,#2253,.T.);
#3845=EDGE_CURVE('',#3179,#3173,#2254,.T.);
#3846=EDGE_CURVE('',#3175,#3180,#2255,.T.);
#3847=EDGE_CURVE('',#3181,#3181,#886,.T.);
#3848=EDGE_CURVE('',#3182,#3182,#887,.T.);
#3849=EDGE_CURVE('',#3183,#3183,#888,.T.);
#3850=EDGE_CURVE('',#3183,#3181,#2256,.T.);
#3851=EDGE_CURVE('',#3184,#3184,#889,.T.);
#3852=EDGE_CURVE('',#3184,#3182,#2257,.T.);
#3853=EDGE_CURVE('',#3185,#3186,#2258,.T.);
#3854=EDGE_CURVE('',#3186,#3187,#2259,.T.);
#3855=EDGE_CURVE('',#3187,#3188,#2260,.T.);
#3856=EDGE_CURVE('',#3185,#3188,#2261,.T.);
#3857=EDGE_CURVE('',#3186,#3189,#2262,.T.);
#3858=EDGE_CURVE('',#3189,#3190,#2263,.T.);
#3859=EDGE_CURVE('',#3190,#3187,#2264,.T.);
#3860=EDGE_CURVE('',#3189,#3191,#2265,.T.);
#3861=EDGE_CURVE('',#3191,#3192,#2266,.T.);
#3862=EDGE_CURVE('',#3192,#3190,#2267,.T.);
#3863=EDGE_CURVE('',#3191,#3193,#2268,.T.);
#3864=EDGE_CURVE('',#3193,#3194,#2269,.T.);
#3865=EDGE_CURVE('',#3194,#3192,#2270,.T.);
#3866=EDGE_CURVE('',#3193,#3195,#2271,.T.);
#3867=EDGE_CURVE('',#3195,#3196,#2272,.T.);
#3868=EDGE_CURVE('',#3196,#3194,#2273,.T.);
#3869=EDGE_CURVE('',#3195,#3185,#2274,.T.);
#3870=EDGE_CURVE('',#3188,#3196,#2275,.T.);
#3871=EDGE_CURVE('',#3197,#3197,#890,.T.);
#3872=EDGE_CURVE('',#3198,#3198,#891,.T.);
#3873=EDGE_CURVE('',#3199,#3199,#892,.T.);
#3874=EDGE_CURVE('',#3199,#3198,#2276,.T.);
#3875=EDGE_CURVE('',#3200,#3200,#893,.T.);
#3876=EDGE_CURVE('',#3200,#3199,#2277,.T.);
#3877=EDGE_CURVE('',#3201,#3201,#894,.T.);
#3878=EDGE_CURVE('',#3201,#3200,#2278,.T.);
#3879=EDGE_CURVE('',#3202,#3202,#895,.T.);
#3880=EDGE_CURVE('',#3203,#3203,#896,.F.);
#3881=EDGE_CURVE('',#3203,#3202,#2279,.T.);
#3882=EDGE_CURVE('',#3197,#3203,#2280,.T.);
#3883=EDGE_CURVE('',#3204,#3204,#897,.T.);
#3884=EDGE_CURVE('',#3204,#3205,#2281,.T.);
#3885=EDGE_CURVE('',#3205,#3205,#898,.T.);
#3886=EDGE_CURVE('',#3206,#3206,#899,.T.);
#3887=EDGE_CURVE('',#3206,#3207,#2282,.T.);
#3888=EDGE_CURVE('',#3207,#3207,#900,.T.);
#3889=EDGE_CURVE('',#3208,#3209,#2283,.T.);
#3890=EDGE_CURVE('',#3208,#3210,#2284,.T.);
#3891=EDGE_CURVE('',#3211,#3210,#2285,.T.);
#3892=EDGE_CURVE('',#3211,#3209,#2286,.T.);
#3893=EDGE_CURVE('',#3209,#3212,#901,.T.);
#3894=EDGE_CURVE('',#3213,#3211,#2287,.T.);
#3895=EDGE_CURVE('',#3212,#3213,#2288,.T.);
#3896=EDGE_CURVE('',#3212,#3214,#2289,.T.);
#3897=EDGE_CURVE('',#3213,#3215,#2290,.T.);
#3898=EDGE_CURVE('',#3215,#3214,#2291,.T.);
#3899=EDGE_CURVE('',#3210,#3215,#2292,.T.);
#3900=EDGE_CURVE('',#3214,#3208,#902,.T.);
#3901=EDGE_CURVE('',#3216,#3217,#2293,.T.);
#3902=EDGE_CURVE('',#3216,#3218,#2294,.T.);
#3903=EDGE_CURVE('',#3219,#3218,#2295,.T.);
#3904=EDGE_CURVE('',#3219,#3217,#2296,.T.);
#3905=EDGE_CURVE('',#3217,#3220,#903,.T.);
#3906=EDGE_CURVE('',#3221,#3219,#2297,.T.);
#3907=EDGE_CURVE('',#3220,#3221,#2298,.T.);
#3908=EDGE_CURVE('',#3220,#3222,#2299,.T.);
#3909=EDGE_CURVE('',#3221,#3223,#2300,.T.);
#3910=EDGE_CURVE('',#3223,#3222,#2301,.T.);
#3911=EDGE_CURVE('',#3218,#3223,#2302,.T.);
#3912=EDGE_CURVE('',#3222,#3216,#904,.T.);
#3913=EDGE_CURVE('',#3224,#3224,#905,.T.);
#3914=EDGE_CURVE('',#3224,#3225,#2303,.T.);
#3915=EDGE_CURVE('',#3225,#3225,#906,.T.);
#3916=EDGE_CURVE('',#3226,#3226,#907,.T.);
#3917=EDGE_CURVE('',#3226,#3227,#2304,.T.);
#3918=EDGE_CURVE('',#3227,#3227,#908,.T.);
#3919=EDGE_CURVE('',#3228,#3228,#909,.T.);
#3920=EDGE_CURVE('',#3228,#3229,#2305,.T.);
#3921=EDGE_CURVE('',#3229,#3229,#910,.T.);
#3922=EDGE_CURVE('',#3230,#3230,#911,.T.);
#3923=EDGE_CURVE('',#3230,#3231,#2306,.T.);
#3924=EDGE_CURVE('',#3231,#3231,#912,.T.);
#3925=EDGE_CURVE('',#3232,#3232,#913,.T.);
#3926=EDGE_CURVE('',#3232,#3233,#2307,.T.);
#3927=EDGE_CURVE('',#3233,#3233,#914,.T.);
#3928=EDGE_CURVE('',#3234,#3234,#915,.T.);
#3929=EDGE_CURVE('',#3234,#3235,#2308,.T.);
#3930=EDGE_CURVE('',#3235,#3235,#916,.T.);
#3931=EDGE_CURVE('',#3236,#3236,#917,.T.);
#3932=EDGE_CURVE('',#3236,#3237,#2309,.T.);
#3933=EDGE_CURVE('',#3237,#3237,#918,.T.);
#3934=EDGE_CURVE('',#3238,#3238,#919,.T.);
#3935=EDGE_CURVE('',#3238,#3239,#2310,.T.);
#3936=EDGE_CURVE('',#3239,#3239,#920,.T.);
#3937=EDGE_CURVE('',#3240,#3240,#921,.T.);
#3938=EDGE_CURVE('',#3240,#3241,#2311,.T.);
#3939=EDGE_CURVE('',#3241,#3241,#922,.T.);
#3940=EDGE_CURVE('',#3242,#3243,#2312,.T.);
#3941=EDGE_CURVE('',#3242,#3244,#2313,.T.);
#3942=EDGE_CURVE('',#3245,#3244,#2314,.T.);
#3943=EDGE_CURVE('',#3243,#3245,#2315,.T.);
#3944=EDGE_CURVE('',#3246,#3242,#2316,.T.);
#3945=EDGE_CURVE('',#3246,#3247,#2317,.T.);
#3946=EDGE_CURVE('',#3244,#3247,#2318,.T.);
#3947=EDGE_CURVE('',#3248,#3246,#2319,.T.);
#3948=EDGE_CURVE('',#3249,#3248,#2320,.T.);
#3949=EDGE_CURVE('',#3247,#3249,#2321,.T.);
#3950=EDGE_CURVE('',#3250,#3250,#923,.T.);
#3951=EDGE_CURVE('',#3249,#3245,#924,.T.);
#3952=EDGE_CURVE('',#3243,#3248,#925,.T.);
#3953=EDGE_CURVE('',#3251,#3251,#926,.T.);
#3954=EDGE_CURVE('',#3251,#3252,#2322,.T.);
#3955=EDGE_CURVE('',#3252,#3252,#927,.T.);
#3956=EDGE_CURVE('',#3250,#3253,#2323,.T.);
#3957=EDGE_CURVE('',#3253,#3253,#928,.T.);
#3958=EDGE_CURVE('',#3254,#3254,#929,.T.);
#3959=EDGE_CURVE('',#3254,#3255,#2324,.T.);
#3960=EDGE_CURVE('',#3255,#3255,#930,.T.);
#3961=EDGE_CURVE('',#3256,#3256,#931,.T.);
#3962=EDGE_CURVE('',#3256,#3257,#2325,.T.);
#3963=EDGE_CURVE('',#3257,#3257,#932,.T.);
#3964=EDGE_CURVE('',#3258,#3259,#2326,.T.);
#3965=EDGE_CURVE('',#3258,#3260,#2327,.T.);
#3966=EDGE_CURVE('',#3261,#3260,#2328,.T.);
#3967=EDGE_CURVE('',#3259,#3261,#2329,.T.);
#3968=EDGE_CURVE('',#3262,#3258,#2330,.T.);
#3969=EDGE_CURVE('',#3262,#3263,#2331,.T.);
#3970=EDGE_CURVE('',#3260,#3263,#2332,.T.);
#3971=EDGE_CURVE('',#3264,#3262,#2333,.T.);
#3972=EDGE_CURVE('',#3265,#3264,#2334,.T.);
#3973=EDGE_CURVE('',#3263,#3265,#2335,.T.);
#3974=EDGE_CURVE('',#3266,#3266,#933,.T.);
#3975=EDGE_CURVE('',#3265,#3261,#934,.T.);
#3976=EDGE_CURVE('',#3264,#3259,#935,.T.);
#3977=EDGE_CURVE('',#3267,#3268,#2336,.T.);
#3978=EDGE_CURVE('',#3269,#3267,#936,.T.);
#3979=EDGE_CURVE('',#3270,#3269,#2337,.T.);
#3980=EDGE_CURVE('',#3270,#3268,#937,.T.);
#3981=EDGE_CURVE('',#3270,#3271,#2338,.T.);
#3982=EDGE_CURVE('',#3272,#3271,#938,.T.);
#3983=EDGE_CURVE('',#3272,#3268,#2339,.T.);
#3984=EDGE_CURVE('',#3273,#3269,#2340,.T.);
#3985=EDGE_CURVE('',#3271,#3273,#2341,.T.);
#3986=EDGE_CURVE('',#3274,#3272,#2342,.T.);
#3987=EDGE_CURVE('',#3267,#3274,#2343,.T.);
#3988=EDGE_CURVE('',#3273,#3274,#939,.T.);
#3989=EDGE_CURVE('',#3266,#3275,#2344,.T.);
#3990=EDGE_CURVE('',#3275,#3275,#940,.T.);
#3991=EDGE_CURVE('',#3276,#3276,#941,.T.);
#3992=EDGE_CURVE('',#3276,#3277,#2345,.T.);
#3993=EDGE_CURVE('',#3277,#3277,#942,.T.);
#3994=EDGE_CURVE('',#3278,#3278,#943,.T.);
#3995=EDGE_CURVE('',#3278,#3279,#2346,.T.);
#3996=EDGE_CURVE('',#3279,#3279,#944,.T.);
#3997=EDGE_CURVE('',#3280,#3280,#945,.T.);
#3998=EDGE_CURVE('',#3280,#3281,#2347,.T.);
#3999=EDGE_CURVE('',#3281,#3281,#946,.T.);
#4000=EDGE_CURVE('',#3282,#3282,#947,.T.);
#4001=EDGE_CURVE('',#3282,#3283,#2348,.T.);
#4002=EDGE_CURVE('',#3283,#3283,#948,.T.);
#4003=EDGE_CURVE('',#3284,#3284,#949,.T.);
#4004=EDGE_CURVE('',#3284,#3285,#2349,.T.);
#4005=EDGE_CURVE('',#3285,#3285,#950,.T.);
#4006=EDGE_CURVE('',#3286,#3286,#951,.T.);
#4007=EDGE_CURVE('',#3286,#3287,#2350,.T.);
#4008=EDGE_CURVE('',#3287,#3287,#952,.T.);
#4009=EDGE_CURVE('',#3288,#3289,#2351,.T.);
#4010=EDGE_CURVE('',#3290,#3288,#2352,.T.);
#4011=EDGE_CURVE('',#3291,#3290,#2353,.T.);
#4012=EDGE_CURVE('',#3292,#3291,#2354,.T.);
#4013=EDGE_CURVE('',#3293,#3292,#2355,.T.);
#4014=EDGE_CURVE('',#3294,#3293,#2356,.T.);
#4015=EDGE_CURVE('',#3295,#3294,#2357,.T.);
#4016=EDGE_CURVE('',#3289,#3295,#2358,.T.);
#4017=EDGE_CURVE('',#3292,#3296,#2359,.T.);
#4018=EDGE_CURVE('',#3296,#3297,#2360,.T.);
#4019=EDGE_CURVE('',#3297,#3293,#2361,.T.);
#4020=EDGE_CURVE('',#3298,#3291,#2362,.T.);
#4021=EDGE_CURVE('',#3298,#3296,#2363,.T.);
#4022=EDGE_CURVE('',#3290,#3299,#2364,.T.);
#4023=EDGE_CURVE('',#3299,#3298,#2365,.T.);
#4024=EDGE_CURVE('',#3300,#3288,#2366,.T.);
#4025=EDGE_CURVE('',#3300,#3299,#2367,.T.);
#4026=EDGE_CURVE('',#3301,#3300,#2368,.T.);
#4027=EDGE_CURVE('',#3302,#3301,#2369,.T.);
#4028=EDGE_CURVE('',#3303,#3302,#2370,.T.);
#4029=EDGE_CURVE('',#3297,#3303,#2371,.T.);
#4030=EDGE_CURVE('',#3289,#3301,#2372,.T.);
#4031=EDGE_CURVE('',#3302,#3295,#2373,.T.);
#4032=EDGE_CURVE('',#3294,#3303,#2374,.T.);
#4033=EDGE_CURVE('',#3304,#3304,#953,.T.);
#4034=EDGE_CURVE('',#3305,#3305,#954,.T.);
#4035=EDGE_CURVE('',#3305,#3304,#2375,.T.);
#4036=EDGE_CURVE('',#3306,#3306,#955,.T.);
#4037=EDGE_CURVE('',#3306,#3305,#2376,.T.);
#4038=EDGE_CURVE('',#3307,#3307,#956,.T.);
#4039=EDGE_CURVE('',#3307,#3306,#2377,.T.);
#4040=EDGE_CURVE('',#3308,#3308,#957,.T.);
#4041=EDGE_CURVE('',#3309,#3309,#958,.F.);
#4042=EDGE_CURVE('',#3309,#3308,#2378,.T.);
#4043=EDGE_CURVE('',#3310,#3310,#959,.F.);
#4044=EDGE_CURVE('',#3310,#3309,#2379,.T.);
#4045=EDGE_CURVE('',#3311,#3311,#960,.T.);
#4046=EDGE_CURVE('',#3311,#3310,#2380,.T.);
#4047=EDGE_CURVE('',#3312,#3313,#2381,.T.);
#4048=EDGE_CURVE('',#3313,#3314,#2382,.T.);
#4049=EDGE_CURVE('',#3314,#3315,#2383,.T.);
#4050=EDGE_CURVE('',#3312,#3315,#2384,.T.);
#4051=EDGE_CURVE('',#3313,#3316,#2385,.T.);
#4052=EDGE_CURVE('',#3316,#3317,#2386,.T.);
#4053=EDGE_CURVE('',#3317,#3314,#2387,.T.);
#4054=EDGE_CURVE('',#3316,#3318,#2388,.T.);
#4055=EDGE_CURVE('',#3318,#3319,#2389,.T.);
#4056=EDGE_CURVE('',#3319,#3317,#2390,.T.);
#4057=EDGE_CURVE('',#3318,#3320,#2391,.T.);
#4058=EDGE_CURVE('',#3320,#3321,#2392,.T.);
#4059=EDGE_CURVE('',#3321,#3319,#2393,.T.);
#4060=EDGE_CURVE('',#3320,#3322,#2394,.T.);
#4061=EDGE_CURVE('',#3322,#3323,#2395,.T.);
#4062=EDGE_CURVE('',#3323,#3321,#2396,.T.);
#4063=EDGE_CURVE('',#3322,#3312,#2397,.T.);
#4064=EDGE_CURVE('',#3315,#3323,#2398,.T.);
#4065=EDGE_CURVE('',#3324,#3324,#961,.T.);
#4066=EDGE_CURVE('',#3324,#3325,#2399,.T.);
#4067=EDGE_CURVE('',#3325,#3325,#962,.T.);
#4068=EDGE_CURVE('',#3326,#3327,#2400,.T.);
#4069=EDGE_CURVE('',#3327,#3328,#2401,.T.);
#4070=EDGE_CURVE('',#3329,#3328,#2402,.T.);
#4071=EDGE_CURVE('',#3326,#3329,#2403,.T.);
#4072=EDGE_CURVE('',#3330,#3326,#2404,.T.);
#4073=EDGE_CURVE('',#3331,#3329,#2405,.T.);
#4074=EDGE_CURVE('',#3330,#3331,#2406,.T.);
#4075=EDGE_CURVE('',#3332,#3330,#2407,.T.);
#4076=EDGE_CURVE('',#3333,#3331,#2408,.T.);
#4077=EDGE_CURVE('',#3332,#3333,#2409,.T.);
#4078=EDGE_CURVE('',#3327,#3332,#2410,.T.);
#4079=EDGE_CURVE('',#3328,#3333,#2411,.T.);
#4080=EDGE_CURVE('',#3334,#3334,#963,.T.);
#4081=EDGE_CURVE('',#3335,#3335,#964,.T.);
#4082=EDGE_CURVE('',#3336,#3336,#965,.T.);
#4083=EDGE_CURVE('',#3336,#3334,#2412,.T.);
#4084=EDGE_CURVE('',#3337,#3337,#966,.T.);
#4085=EDGE_CURVE('',#3337,#3338,#2413,.T.);
#4086=EDGE_CURVE('',#3338,#3338,#967,.T.);
#4087=EDGE_CURVE('',#3335,#3339,#2414,.T.);
#4088=EDGE_CURVE('',#3339,#3339,#968,.T.);
#4089=EDGE_CURVE('',#3340,#3340,#969,.T.);
#4090=EDGE_CURVE('',#3340,#3341,#2415,.T.);
#4091=EDGE_CURVE('',#3341,#3341,#970,.T.);
#4092=EDGE_CURVE('',#3342,#3342,#971,.T.);
#4093=EDGE_CURVE('',#3342,#3343,#2416,.T.);
#4094=EDGE_CURVE('',#3343,#3343,#972,.T.);
#4095=ORIENTED_EDGE('',*,*,#3344,.F.);
#4096=ORIENTED_EDGE('',*,*,#3345,.F.);
#4097=ORIENTED_EDGE('',*,*,#3346,.F.);
#4098=ORIENTED_EDGE('',*,*,#3347,.T.);
#4099=ORIENTED_EDGE('',*,*,#3348,.F.);
#4100=ORIENTED_EDGE('',*,*,#3347,.F.);
#4101=ORIENTED_EDGE('',*,*,#3349,.F.);
#4102=ORIENTED_EDGE('',*,*,#3350,.T.);
#4103=ORIENTED_EDGE('',*,*,#3351,.F.);
#4104=ORIENTED_EDGE('',*,*,#3350,.F.);
#4105=ORIENTED_EDGE('',*,*,#3352,.F.);
#4106=ORIENTED_EDGE('',*,*,#3353,.T.);
#4107=ORIENTED_EDGE('',*,*,#3354,.F.);
#4108=ORIENTED_EDGE('',*,*,#3353,.F.);
#4109=ORIENTED_EDGE('',*,*,#3355,.F.);
#4110=ORIENTED_EDGE('',*,*,#3345,.T.);
#4111=ORIENTED_EDGE('',*,*,#3349,.T.);
#4112=ORIENTED_EDGE('',*,*,#3346,.T.);
#4113=ORIENTED_EDGE('',*,*,#3355,.T.);
#4114=ORIENTED_EDGE('',*,*,#3352,.T.);
#4115=ORIENTED_EDGE('',*,*,#3356,.F.);
#4116=ORIENTED_EDGE('',*,*,#3357,.T.);
#4117=ORIENTED_EDGE('',*,*,#3358,.F.);
#4118=ORIENTED_EDGE('',*,*,#3357,.F.);
#4119=ORIENTED_EDGE('',*,*,#3359,.F.);
#4120=ORIENTED_EDGE('',*,*,#3360,.T.);
#4121=ORIENTED_EDGE('',*,*,#3361,.F.);
#4122=ORIENTED_EDGE('',*,*,#3360,.F.);
#4123=ORIENTED_EDGE('',*,*,#3362,.F.);
#4124=ORIENTED_EDGE('',*,*,#3363,.T.);
#4125=ORIENTED_EDGE('',*,*,#3364,.F.);
#4126=ORIENTED_EDGE('',*,*,#3363,.F.);
#4127=ORIENTED_EDGE('',*,*,#3365,.F.);
#4128=ORIENTED_EDGE('',*,*,#3366,.T.);
#4129=ORIENTED_EDGE('',*,*,#3367,.F.);
#4130=ORIENTED_EDGE('',*,*,#3366,.F.);
#4131=ORIENTED_EDGE('',*,*,#3368,.F.);
#4132=ORIENTED_EDGE('',*,*,#3369,.T.);
#4133=ORIENTED_EDGE('',*,*,#3370,.F.);
#4134=ORIENTED_EDGE('',*,*,#3369,.F.);
#4135=ORIENTED_EDGE('',*,*,#3371,.F.);
#4136=ORIENTED_EDGE('',*,*,#3372,.T.);
#4137=ORIENTED_EDGE('',*,*,#3373,.F.);
#4138=ORIENTED_EDGE('',*,*,#3372,.F.);
#4139=ORIENTED_EDGE('',*,*,#3374,.T.);
#4140=ORIENTED_EDGE('',*,*,#3375,.T.);
#4141=ORIENTED_EDGE('',*,*,#3376,.F.);
#4142=ORIENTED_EDGE('',*,*,#3377,.F.);
#4143=ORIENTED_EDGE('',*,*,#3378,.T.);
#4144=ORIENTED_EDGE('',*,*,#3377,.T.);
#4145=ORIENTED_EDGE('',*,*,#3379,.F.);
#4146=ORIENTED_EDGE('',*,*,#3380,.F.);
#4147=ORIENTED_EDGE('',*,*,#3381,.T.);
#4148=ORIENTED_EDGE('',*,*,#3380,.T.);
#4149=ORIENTED_EDGE('',*,*,#3382,.F.);
#4150=ORIENTED_EDGE('',*,*,#3383,.F.);
#4151=ORIENTED_EDGE('',*,*,#3384,.T.);
#4152=ORIENTED_EDGE('',*,*,#3383,.T.);
#4153=ORIENTED_EDGE('',*,*,#3385,.F.);
#4154=ORIENTED_EDGE('',*,*,#3375,.F.);
#4155=ORIENTED_EDGE('',*,*,#3385,.T.);
#4156=ORIENTED_EDGE('',*,*,#3382,.T.);
#4157=ORIENTED_EDGE('',*,*,#3379,.T.);
#4158=ORIENTED_EDGE('',*,*,#3376,.T.);
#4159=ORIENTED_EDGE('',*,*,#3351,.T.);
#4160=ORIENTED_EDGE('',*,*,#3354,.T.);
#4161=ORIENTED_EDGE('',*,*,#3344,.T.);
#4162=ORIENTED_EDGE('',*,*,#3348,.T.);
#4163=ORIENTED_EDGE('',*,*,#3358,.T.);
#4164=ORIENTED_EDGE('',*,*,#3361,.T.);
#4165=ORIENTED_EDGE('',*,*,#3364,.T.);
#4166=ORIENTED_EDGE('',*,*,#3367,.T.);
#4167=ORIENTED_EDGE('',*,*,#3370,.T.);
#4168=ORIENTED_EDGE('',*,*,#3373,.T.);
#4169=ORIENTED_EDGE('',*,*,#3384,.F.);
#4170=ORIENTED_EDGE('',*,*,#3374,.F.);
#4171=ORIENTED_EDGE('',*,*,#3378,.F.);
#4172=ORIENTED_EDGE('',*,*,#3381,.F.);
#4173=ORIENTED_EDGE('',*,*,#3356,.T.);
#4174=ORIENTED_EDGE('',*,*,#3359,.T.);
#4175=ORIENTED_EDGE('',*,*,#3362,.T.);
#4176=ORIENTED_EDGE('',*,*,#3365,.T.);
#4177=ORIENTED_EDGE('',*,*,#3368,.T.);
#4178=ORIENTED_EDGE('',*,*,#3371,.T.);
#4179=ORIENTED_EDGE('',*,*,#3386,.T.);
#4180=ORIENTED_EDGE('',*,*,#3387,.T.);
#4181=ORIENTED_EDGE('',*,*,#3388,.F.);
#4182=ORIENTED_EDGE('',*,*,#3389,.F.);
#4183=ORIENTED_EDGE('',*,*,#3390,.T.);
#4184=ORIENTED_EDGE('',*,*,#3389,.T.);
#4185=ORIENTED_EDGE('',*,*,#3391,.F.);
#4186=ORIENTED_EDGE('',*,*,#3392,.F.);
#4187=ORIENTED_EDGE('',*,*,#3393,.T.);
#4188=ORIENTED_EDGE('',*,*,#3392,.T.);
#4189=ORIENTED_EDGE('',*,*,#3394,.F.);
#4190=ORIENTED_EDGE('',*,*,#3395,.F.);
#4191=ORIENTED_EDGE('',*,*,#3396,.T.);
#4192=ORIENTED_EDGE('',*,*,#3395,.T.);
#4193=ORIENTED_EDGE('',*,*,#3397,.F.);
#4194=ORIENTED_EDGE('',*,*,#3387,.F.);
#4195=ORIENTED_EDGE('',*,*,#3397,.T.);
#4196=ORIENTED_EDGE('',*,*,#3394,.T.);
#4197=ORIENTED_EDGE('',*,*,#3391,.T.);
#4198=ORIENTED_EDGE('',*,*,#3388,.T.);
#4199=ORIENTED_EDGE('',*,*,#3396,.F.);
#4200=ORIENTED_EDGE('',*,*,#3386,.F.);
#4201=ORIENTED_EDGE('',*,*,#3390,.F.);
#4202=ORIENTED_EDGE('',*,*,#3393,.F.);
#4203=ORIENTED_EDGE('',*,*,#3398,.T.);
#4204=ORIENTED_EDGE('',*,*,#3399,.T.);
#4205=ORIENTED_EDGE('',*,*,#3400,.F.);
#4206=ORIENTED_EDGE('',*,*,#3401,.F.);
#4207=ORIENTED_EDGE('',*,*,#3402,.T.);
#4208=ORIENTED_EDGE('',*,*,#3401,.T.);
#4209=ORIENTED_EDGE('',*,*,#3403,.F.);
#4210=ORIENTED_EDGE('',*,*,#3404,.F.);
#4211=ORIENTED_EDGE('',*,*,#3405,.T.);
#4212=ORIENTED_EDGE('',*,*,#3404,.T.);
#4213=ORIENTED_EDGE('',*,*,#3406,.F.);
#4214=ORIENTED_EDGE('',*,*,#3407,.F.);
#4215=ORIENTED_EDGE('',*,*,#3408,.T.);
#4216=ORIENTED_EDGE('',*,*,#3407,.T.);
#4217=ORIENTED_EDGE('',*,*,#3409,.F.);
#4218=ORIENTED_EDGE('',*,*,#3399,.F.);
#4219=ORIENTED_EDGE('',*,*,#3409,.T.);
#4220=ORIENTED_EDGE('',*,*,#3406,.T.);
#4221=ORIENTED_EDGE('',*,*,#3403,.T.);
#4222=ORIENTED_EDGE('',*,*,#3400,.T.);
#4223=ORIENTED_EDGE('',*,*,#3408,.F.);
#4224=ORIENTED_EDGE('',*,*,#3398,.F.);
#4225=ORIENTED_EDGE('',*,*,#3402,.F.);
#4226=ORIENTED_EDGE('',*,*,#3405,.F.);
#4227=ORIENTED_EDGE('',*,*,#3410,.F.);
#4228=ORIENTED_EDGE('',*,*,#3411,.T.);
#4229=ORIENTED_EDGE('',*,*,#3412,.F.);
#4230=ORIENTED_EDGE('',*,*,#3411,.F.);
#4231=ORIENTED_EDGE('',*,*,#3413,.F.);
#4232=ORIENTED_EDGE('',*,*,#3414,.T.);
#4233=ORIENTED_EDGE('',*,*,#3415,.F.);
#4234=ORIENTED_EDGE('',*,*,#3414,.F.);
#4235=ORIENTED_EDGE('',*,*,#3416,.F.);
#4236=ORIENTED_EDGE('',*,*,#3417,.T.);
#4237=ORIENTED_EDGE('',*,*,#3418,.F.);
#4238=ORIENTED_EDGE('',*,*,#3417,.F.);
#4239=ORIENTED_EDGE('',*,*,#3419,.F.);
#4240=ORIENTED_EDGE('',*,*,#3420,.T.);
#4241=ORIENTED_EDGE('',*,*,#3421,.F.);
#4242=ORIENTED_EDGE('',*,*,#3420,.F.);
#4243=ORIENTED_EDGE('',*,*,#3422,.F.);
#4244=ORIENTED_EDGE('',*,*,#3423,.T.);
#4245=ORIENTED_EDGE('',*,*,#3424,.F.);
#4246=ORIENTED_EDGE('',*,*,#3423,.F.);
#4247=ORIENTED_EDGE('',*,*,#3425,.F.);
#4248=ORIENTED_EDGE('',*,*,#3426,.T.);
#4249=ORIENTED_EDGE('',*,*,#3427,.F.);
#4250=ORIENTED_EDGE('',*,*,#3426,.F.);
#4251=ORIENTED_EDGE('',*,*,#3428,.F.);
#4252=ORIENTED_EDGE('',*,*,#3429,.T.);
#4253=ORIENTED_EDGE('',*,*,#3430,.F.);
#4254=ORIENTED_EDGE('',*,*,#3429,.F.);
#4255=ORIENTED_EDGE('',*,*,#3431,.F.);
#4256=ORIENTED_EDGE('',*,*,#3432,.F.);
#4257=ORIENTED_EDGE('',*,*,#3433,.T.);
#4258=ORIENTED_EDGE('',*,*,#3434,.F.);
#4259=ORIENTED_EDGE('',*,*,#3415,.T.);
#4260=ORIENTED_EDGE('',*,*,#3435,.F.);
#4261=ORIENTED_EDGE('',*,*,#3436,.F.);
#4262=ORIENTED_EDGE('',*,*,#3437,.F.);
#4263=ORIENTED_EDGE('',*,*,#3438,.F.);
#4264=ORIENTED_EDGE('',*,*,#3412,.T.);
#4265=ORIENTED_EDGE('',*,*,#3439,.F.);
#4266=ORIENTED_EDGE('',*,*,#3437,.T.);
#4267=ORIENTED_EDGE('',*,*,#3440,.F.);
#4268=ORIENTED_EDGE('',*,*,#3441,.F.);
#4269=ORIENTED_EDGE('',*,*,#3442,.F.);
#4270=ORIENTED_EDGE('',*,*,#3443,.T.);
#4271=ORIENTED_EDGE('',*,*,#3444,.F.);
#4272=ORIENTED_EDGE('',*,*,#3433,.F.);
#4273=ORIENTED_EDGE('',*,*,#3445,.T.);
#4274=ORIENTED_EDGE('',*,*,#3446,.F.);
#4275=ORIENTED_EDGE('',*,*,#3447,.F.);
#4276=ORIENTED_EDGE('',*,*,#3438,.T.);
#4277=ORIENTED_EDGE('',*,*,#3439,.T.);
#4278=ORIENTED_EDGE('',*,*,#3448,.T.);
#4279=ORIENTED_EDGE('',*,*,#3442,.T.);
#4280=ORIENTED_EDGE('',*,*,#3432,.T.);
#4281=ORIENTED_EDGE('',*,*,#3428,.T.);
#4282=ORIENTED_EDGE('',*,*,#3425,.T.);
#4283=ORIENTED_EDGE('',*,*,#3422,.T.);
#4284=ORIENTED_EDGE('',*,*,#3419,.T.);
#4285=ORIENTED_EDGE('',*,*,#3416,.T.);
#4286=ORIENTED_EDGE('',*,*,#3431,.T.);
#4287=ORIENTED_EDGE('',*,*,#3449,.T.);
#4288=ORIENTED_EDGE('',*,*,#3450,.F.);
#4289=ORIENTED_EDGE('',*,*,#3445,.F.);
#4290=ORIENTED_EDGE('',*,*,#3451,.T.);
#4291=ORIENTED_EDGE('',*,*,#3452,.F.);
#4292=ORIENTED_EDGE('',*,*,#3449,.F.);
#4293=ORIENTED_EDGE('',*,*,#3434,.T.);
#4294=ORIENTED_EDGE('',*,*,#3444,.T.);
#4295=ORIENTED_EDGE('',*,*,#3453,.T.);
#4296=ORIENTED_EDGE('',*,*,#3440,.T.);
#4297=ORIENTED_EDGE('',*,*,#3436,.T.);
#4298=ORIENTED_EDGE('',*,*,#3430,.T.);
#4299=ORIENTED_EDGE('',*,*,#3427,.T.);
#4300=ORIENTED_EDGE('',*,*,#3424,.T.);
#4301=ORIENTED_EDGE('',*,*,#3421,.T.);
#4302=ORIENTED_EDGE('',*,*,#3418,.T.);
#4303=ORIENTED_EDGE('',*,*,#3435,.T.);
#4304=ORIENTED_EDGE('',*,*,#3447,.T.);
#4305=ORIENTED_EDGE('',*,*,#3454,.F.);
#4306=ORIENTED_EDGE('',*,*,#3451,.F.);
#4307=ORIENTED_EDGE('',*,*,#3454,.T.);
#4308=ORIENTED_EDGE('',*,*,#3446,.T.);
#4309=ORIENTED_EDGE('',*,*,#3450,.T.);
#4310=ORIENTED_EDGE('',*,*,#3452,.T.);
#4311=ORIENTED_EDGE('',*,*,#3453,.F.);
#4312=ORIENTED_EDGE('',*,*,#3443,.F.);
#4313=ORIENTED_EDGE('',*,*,#3448,.F.);
#4314=ORIENTED_EDGE('',*,*,#3441,.T.);
#4315=ORIENTED_EDGE('',*,*,#3410,.T.);
#4316=ORIENTED_EDGE('',*,*,#3413,.T.);
#4317=ORIENTED_EDGE('',*,*,#3455,.F.);
#4318=ORIENTED_EDGE('',*,*,#3456,.T.);
#4319=ORIENTED_EDGE('',*,*,#3457,.F.);
#4320=ORIENTED_EDGE('',*,*,#3456,.F.);
#4321=ORIENTED_EDGE('',*,*,#3458,.F.);
#4322=ORIENTED_EDGE('',*,*,#3459,.T.);
#4323=ORIENTED_EDGE('',*,*,#3460,.F.);
#4324=ORIENTED_EDGE('',*,*,#3459,.F.);
#4325=ORIENTED_EDGE('',*,*,#3461,.F.);
#4326=ORIENTED_EDGE('',*,*,#3462,.T.);
#4327=ORIENTED_EDGE('',*,*,#3463,.F.);
#4328=ORIENTED_EDGE('',*,*,#3462,.F.);
#4329=ORIENTED_EDGE('',*,*,#3464,.F.);
#4330=ORIENTED_EDGE('',*,*,#3465,.T.);
#4331=ORIENTED_EDGE('',*,*,#3466,.F.);
#4332=ORIENTED_EDGE('',*,*,#3465,.F.);
#4333=ORIENTED_EDGE('',*,*,#3467,.F.);
#4334=ORIENTED_EDGE('',*,*,#3468,.T.);
#4335=ORIENTED_EDGE('',*,*,#3469,.F.);
#4336=ORIENTED_EDGE('',*,*,#3468,.F.);
#4337=ORIENTED_EDGE('',*,*,#3467,.T.);
#4338=ORIENTED_EDGE('',*,*,#3470,.T.);
#4339=ORIENTED_EDGE('',*,*,#3470,.F.);
#4340=ORIENTED_EDGE('',*,*,#3471,.T.);
#4341=ORIENTED_EDGE('',*,*,#3472,.T.);
#4342=ORIENTED_EDGE('',*,*,#3471,.F.);
#4343=ORIENTED_EDGE('',*,*,#3473,.F.);
#4344=ORIENTED_EDGE('',*,*,#3474,.T.);
#4345=ORIENTED_EDGE('',*,*,#3475,.T.);
#4346=ORIENTED_EDGE('',*,*,#3474,.F.);
#4347=ORIENTED_EDGE('',*,*,#3473,.T.);
#4348=ORIENTED_EDGE('',*,*,#3469,.T.);
#4349=ORIENTED_EDGE('',*,*,#3466,.T.);
#4350=ORIENTED_EDGE('',*,*,#3463,.T.);
#4351=ORIENTED_EDGE('',*,*,#3460,.T.);
#4352=ORIENTED_EDGE('',*,*,#3457,.T.);
#4353=ORIENTED_EDGE('',*,*,#3475,.F.);
#4354=ORIENTED_EDGE('',*,*,#3472,.F.);
#4355=ORIENTED_EDGE('',*,*,#3464,.T.);
#4356=ORIENTED_EDGE('',*,*,#3461,.T.);
#4357=ORIENTED_EDGE('',*,*,#3458,.T.);
#4358=ORIENTED_EDGE('',*,*,#3455,.T.);
#4359=ORIENTED_EDGE('',*,*,#3476,.F.);
#4360=ORIENTED_EDGE('',*,*,#3477,.T.);
#4361=ORIENTED_EDGE('',*,*,#3478,.F.);
#4362=ORIENTED_EDGE('',*,*,#3477,.F.);
#4363=ORIENTED_EDGE('',*,*,#3479,.F.);
#4364=ORIENTED_EDGE('',*,*,#3480,.T.);
#4365=ORIENTED_EDGE('',*,*,#3481,.F.);
#4366=ORIENTED_EDGE('',*,*,#3480,.F.);
#4367=ORIENTED_EDGE('',*,*,#3482,.F.);
#4368=ORIENTED_EDGE('',*,*,#3483,.T.);
#4369=ORIENTED_EDGE('',*,*,#3484,.F.);
#4370=ORIENTED_EDGE('',*,*,#3483,.F.);
#4371=ORIENTED_EDGE('',*,*,#3485,.F.);
#4372=ORIENTED_EDGE('',*,*,#3486,.T.);
#4373=ORIENTED_EDGE('',*,*,#3487,.F.);
#4374=ORIENTED_EDGE('',*,*,#3486,.F.);
#4375=ORIENTED_EDGE('',*,*,#3488,.F.);
#4376=ORIENTED_EDGE('',*,*,#3489,.T.);
#4377=ORIENTED_EDGE('',*,*,#3490,.T.);
#4378=ORIENTED_EDGE('',*,*,#3489,.F.);
#4379=ORIENTED_EDGE('',*,*,#3490,.F.);
#4380=ORIENTED_EDGE('',*,*,#3491,.F.);
#4381=ORIENTED_EDGE('',*,*,#3492,.F.);
#4382=ORIENTED_EDGE('',*,*,#3493,.T.);
#4383=ORIENTED_EDGE('',*,*,#3491,.T.);
#4384=ORIENTED_EDGE('',*,*,#3493,.F.);
#4385=ORIENTED_EDGE('',*,*,#3494,.F.);
#4386=ORIENTED_EDGE('',*,*,#3495,.T.);
#4387=ORIENTED_EDGE('',*,*,#3496,.T.);
#4388=ORIENTED_EDGE('',*,*,#3495,.F.);
#4389=ORIENTED_EDGE('',*,*,#3494,.T.);
#4390=ORIENTED_EDGE('',*,*,#3492,.T.);
#4391=ORIENTED_EDGE('',*,*,#3487,.T.);
#4392=ORIENTED_EDGE('',*,*,#3484,.T.);
#4393=ORIENTED_EDGE('',*,*,#3481,.T.);
#4394=ORIENTED_EDGE('',*,*,#3478,.T.);
#4395=ORIENTED_EDGE('',*,*,#3496,.F.);
#4396=ORIENTED_EDGE('',*,*,#3488,.T.);
#4397=ORIENTED_EDGE('',*,*,#3485,.T.);
#4398=ORIENTED_EDGE('',*,*,#3482,.T.);
#4399=ORIENTED_EDGE('',*,*,#3479,.T.);
#4400=ORIENTED_EDGE('',*,*,#3476,.T.);
#4401=ORIENTED_EDGE('',*,*,#3497,.F.);
#4402=ORIENTED_EDGE('',*,*,#3498,.T.);
#4403=ORIENTED_EDGE('',*,*,#3499,.F.);
#4404=ORIENTED_EDGE('',*,*,#3498,.F.);
#4405=ORIENTED_EDGE('',*,*,#3500,.F.);
#4406=ORIENTED_EDGE('',*,*,#3501,.T.);
#4407=ORIENTED_EDGE('',*,*,#3502,.F.);
#4408=ORIENTED_EDGE('',*,*,#3501,.F.);
#4409=ORIENTED_EDGE('',*,*,#3503,.F.);
#4410=ORIENTED_EDGE('',*,*,#3504,.T.);
#4411=ORIENTED_EDGE('',*,*,#3505,.F.);
#4412=ORIENTED_EDGE('',*,*,#3504,.F.);
#4413=ORIENTED_EDGE('',*,*,#3506,.F.);
#4414=ORIENTED_EDGE('',*,*,#3507,.T.);
#4415=ORIENTED_EDGE('',*,*,#3508,.F.);
#4416=ORIENTED_EDGE('',*,*,#3507,.F.);
#4417=ORIENTED_EDGE('',*,*,#3509,.F.);
#4418=ORIENTED_EDGE('',*,*,#3510,.T.);
#4419=ORIENTED_EDGE('',*,*,#3511,.F.);
#4420=ORIENTED_EDGE('',*,*,#3510,.F.);
#4421=ORIENTED_EDGE('',*,*,#3512,.F.);
#4422=ORIENTED_EDGE('',*,*,#3513,.T.);
#4423=ORIENTED_EDGE('',*,*,#3514,.F.);
#4424=ORIENTED_EDGE('',*,*,#3513,.F.);
#4425=ORIENTED_EDGE('',*,*,#3515,.F.);
#4426=ORIENTED_EDGE('',*,*,#3516,.T.);
#4427=ORIENTED_EDGE('',*,*,#3517,.F.);
#4428=ORIENTED_EDGE('',*,*,#3516,.F.);
#4429=ORIENTED_EDGE('',*,*,#3518,.F.);
#4430=ORIENTED_EDGE('',*,*,#3519,.F.);
#4431=ORIENTED_EDGE('',*,*,#3520,.T.);
#4432=ORIENTED_EDGE('',*,*,#3521,.F.);
#4433=ORIENTED_EDGE('',*,*,#3502,.T.);
#4434=ORIENTED_EDGE('',*,*,#3522,.F.);
#4435=ORIENTED_EDGE('',*,*,#3523,.F.);
#4436=ORIENTED_EDGE('',*,*,#3524,.F.);
#4437=ORIENTED_EDGE('',*,*,#3525,.F.);
#4438=ORIENTED_EDGE('',*,*,#3499,.T.);
#4439=ORIENTED_EDGE('',*,*,#3526,.F.);
#4440=ORIENTED_EDGE('',*,*,#3524,.T.);
#4441=ORIENTED_EDGE('',*,*,#3527,.F.);
#4442=ORIENTED_EDGE('',*,*,#3528,.F.);
#4443=ORIENTED_EDGE('',*,*,#3529,.F.);
#4444=ORIENTED_EDGE('',*,*,#3530,.T.);
#4445=ORIENTED_EDGE('',*,*,#3531,.F.);
#4446=ORIENTED_EDGE('',*,*,#3520,.F.);
#4447=ORIENTED_EDGE('',*,*,#3532,.T.);
#4448=ORIENTED_EDGE('',*,*,#3533,.F.);
#4449=ORIENTED_EDGE('',*,*,#3534,.F.);
#4450=ORIENTED_EDGE('',*,*,#3525,.T.);
#4451=ORIENTED_EDGE('',*,*,#3526,.T.);
#4452=ORIENTED_EDGE('',*,*,#3535,.T.);
#4453=ORIENTED_EDGE('',*,*,#3529,.T.);
#4454=ORIENTED_EDGE('',*,*,#3519,.T.);
#4455=ORIENTED_EDGE('',*,*,#3515,.T.);
#4456=ORIENTED_EDGE('',*,*,#3512,.T.);
#4457=ORIENTED_EDGE('',*,*,#3509,.T.);
#4458=ORIENTED_EDGE('',*,*,#3506,.T.);
#4459=ORIENTED_EDGE('',*,*,#3503,.T.);
#4460=ORIENTED_EDGE('',*,*,#3518,.T.);
#4461=ORIENTED_EDGE('',*,*,#3536,.T.);
#4462=ORIENTED_EDGE('',*,*,#3537,.F.);
#4463=ORIENTED_EDGE('',*,*,#3532,.F.);
#4464=ORIENTED_EDGE('',*,*,#3538,.T.);
#4465=ORIENTED_EDGE('',*,*,#3539,.F.);
#4466=ORIENTED_EDGE('',*,*,#3536,.F.);
#4467=ORIENTED_EDGE('',*,*,#3521,.T.);
#4468=ORIENTED_EDGE('',*,*,#3531,.T.);
#4469=ORIENTED_EDGE('',*,*,#3540,.T.);
#4470=ORIENTED_EDGE('',*,*,#3527,.T.);
#4471=ORIENTED_EDGE('',*,*,#3523,.T.);
#4472=ORIENTED_EDGE('',*,*,#3517,.T.);
#4473=ORIENTED_EDGE('',*,*,#3514,.T.);
#4474=ORIENTED_EDGE('',*,*,#3511,.T.);
#4475=ORIENTED_EDGE('',*,*,#3508,.T.);
#4476=ORIENTED_EDGE('',*,*,#3505,.T.);
#4477=ORIENTED_EDGE('',*,*,#3522,.T.);
#4478=ORIENTED_EDGE('',*,*,#3534,.T.);
#4479=ORIENTED_EDGE('',*,*,#3541,.F.);
#4480=ORIENTED_EDGE('',*,*,#3538,.F.);
#4481=ORIENTED_EDGE('',*,*,#3541,.T.);
#4482=ORIENTED_EDGE('',*,*,#3533,.T.);
#4483=ORIENTED_EDGE('',*,*,#3537,.T.);
#4484=ORIENTED_EDGE('',*,*,#3539,.T.);
#4485=ORIENTED_EDGE('',*,*,#3540,.F.);
#4486=ORIENTED_EDGE('',*,*,#3530,.F.);
#4487=ORIENTED_EDGE('',*,*,#3535,.F.);
#4488=ORIENTED_EDGE('',*,*,#3528,.T.);
#4489=ORIENTED_EDGE('',*,*,#3497,.T.);
#4490=ORIENTED_EDGE('',*,*,#3500,.T.);
#4491=ORIENTED_EDGE('',*,*,#3542,.F.);
#4492=ORIENTED_EDGE('',*,*,#3543,.T.);
#4493=ORIENTED_EDGE('',*,*,#3544,.F.);
#4494=ORIENTED_EDGE('',*,*,#3543,.F.);
#4495=ORIENTED_EDGE('',*,*,#3545,.F.);
#4496=ORIENTED_EDGE('',*,*,#3546,.T.);
#4497=ORIENTED_EDGE('',*,*,#3547,.F.);
#4498=ORIENTED_EDGE('',*,*,#3546,.F.);
#4499=ORIENTED_EDGE('',*,*,#3548,.F.);
#4500=ORIENTED_EDGE('',*,*,#3549,.T.);
#4501=ORIENTED_EDGE('',*,*,#3550,.F.);
#4502=ORIENTED_EDGE('',*,*,#3549,.F.);
#4503=ORIENTED_EDGE('',*,*,#3551,.F.);
#4504=ORIENTED_EDGE('',*,*,#3552,.T.);
#4505=ORIENTED_EDGE('',*,*,#3553,.F.);
#4506=ORIENTED_EDGE('',*,*,#3552,.F.);
#4507=ORIENTED_EDGE('',*,*,#3554,.F.);
#4508=ORIENTED_EDGE('',*,*,#3555,.T.);
#4509=ORIENTED_EDGE('',*,*,#3556,.F.);
#4510=ORIENTED_EDGE('',*,*,#3555,.F.);
#4511=ORIENTED_EDGE('',*,*,#3554,.T.);
#4512=ORIENTED_EDGE('',*,*,#3557,.T.);
#4513=ORIENTED_EDGE('',*,*,#3557,.F.);
#4514=ORIENTED_EDGE('',*,*,#3558,.T.);
#4515=ORIENTED_EDGE('',*,*,#3559,.T.);
#4516=ORIENTED_EDGE('',*,*,#3558,.F.);
#4517=ORIENTED_EDGE('',*,*,#3560,.F.);
#4518=ORIENTED_EDGE('',*,*,#3561,.T.);
#4519=ORIENTED_EDGE('',*,*,#3562,.T.);
#4520=ORIENTED_EDGE('',*,*,#3561,.F.);
#4521=ORIENTED_EDGE('',*,*,#3560,.T.);
#4522=ORIENTED_EDGE('',*,*,#3556,.T.);
#4523=ORIENTED_EDGE('',*,*,#3553,.T.);
#4524=ORIENTED_EDGE('',*,*,#3550,.T.);
#4525=ORIENTED_EDGE('',*,*,#3547,.T.);
#4526=ORIENTED_EDGE('',*,*,#3544,.T.);
#4527=ORIENTED_EDGE('',*,*,#3562,.F.);
#4528=ORIENTED_EDGE('',*,*,#3559,.F.);
#4529=ORIENTED_EDGE('',*,*,#3551,.T.);
#4530=ORIENTED_EDGE('',*,*,#3548,.T.);
#4531=ORIENTED_EDGE('',*,*,#3545,.T.);
#4532=ORIENTED_EDGE('',*,*,#3542,.T.);
#4533=ORIENTED_EDGE('',*,*,#3563,.F.);
#4534=ORIENTED_EDGE('',*,*,#3564,.T.);
#4535=ORIENTED_EDGE('',*,*,#3565,.F.);
#4536=ORIENTED_EDGE('',*,*,#3564,.F.);
#4537=ORIENTED_EDGE('',*,*,#3566,.F.);
#4538=ORIENTED_EDGE('',*,*,#3567,.T.);
#4539=ORIENTED_EDGE('',*,*,#3568,.F.);
#4540=ORIENTED_EDGE('',*,*,#3567,.F.);
#4541=ORIENTED_EDGE('',*,*,#3569,.F.);
#4542=ORIENTED_EDGE('',*,*,#3570,.T.);
#4543=ORIENTED_EDGE('',*,*,#3571,.F.);
#4544=ORIENTED_EDGE('',*,*,#3570,.F.);
#4545=ORIENTED_EDGE('',*,*,#3572,.F.);
#4546=ORIENTED_EDGE('',*,*,#3573,.T.);
#4547=ORIENTED_EDGE('',*,*,#3574,.F.);
#4548=ORIENTED_EDGE('',*,*,#3573,.F.);
#4549=ORIENTED_EDGE('',*,*,#3575,.F.);
#4550=ORIENTED_EDGE('',*,*,#3576,.T.);
#4551=ORIENTED_EDGE('',*,*,#3577,.T.);
#4552=ORIENTED_EDGE('',*,*,#3576,.F.);
#4553=ORIENTED_EDGE('',*,*,#3577,.F.);
#4554=ORIENTED_EDGE('',*,*,#3578,.F.);
#4555=ORIENTED_EDGE('',*,*,#3579,.F.);
#4556=ORIENTED_EDGE('',*,*,#3580,.T.);
#4557=ORIENTED_EDGE('',*,*,#3578,.T.);
#4558=ORIENTED_EDGE('',*,*,#3580,.F.);
#4559=ORIENTED_EDGE('',*,*,#3581,.F.);
#4560=ORIENTED_EDGE('',*,*,#3582,.T.);
#4561=ORIENTED_EDGE('',*,*,#3583,.T.);
#4562=ORIENTED_EDGE('',*,*,#3582,.F.);
#4563=ORIENTED_EDGE('',*,*,#3581,.T.);
#4564=ORIENTED_EDGE('',*,*,#3579,.T.);
#4565=ORIENTED_EDGE('',*,*,#3574,.T.);
#4566=ORIENTED_EDGE('',*,*,#3571,.T.);
#4567=ORIENTED_EDGE('',*,*,#3568,.T.);
#4568=ORIENTED_EDGE('',*,*,#3565,.T.);
#4569=ORIENTED_EDGE('',*,*,#3583,.F.);
#4570=ORIENTED_EDGE('',*,*,#3575,.T.);
#4571=ORIENTED_EDGE('',*,*,#3572,.T.);
#4572=ORIENTED_EDGE('',*,*,#3569,.T.);
#4573=ORIENTED_EDGE('',*,*,#3566,.T.);
#4574=ORIENTED_EDGE('',*,*,#3563,.T.);
#4575=ORIENTED_EDGE('',*,*,#3584,.F.);
#4576=ORIENTED_EDGE('',*,*,#3585,.T.);
#4577=ORIENTED_EDGE('',*,*,#3586,.F.);
#4578=ORIENTED_EDGE('',*,*,#3585,.F.);
#4579=ORIENTED_EDGE('',*,*,#3584,.T.);
#4580=ORIENTED_EDGE('',*,*,#3587,.F.);
#4581=ORIENTED_EDGE('',*,*,#3588,.T.);
#4582=ORIENTED_EDGE('',*,*,#3589,.F.);
#4583=ORIENTED_EDGE('',*,*,#3588,.F.);
#4584=ORIENTED_EDGE('',*,*,#3587,.T.);
#4585=ORIENTED_EDGE('',*,*,#3590,.F.);
#4586=ORIENTED_EDGE('',*,*,#3591,.T.);
#4587=ORIENTED_EDGE('',*,*,#3592,.F.);
#4588=ORIENTED_EDGE('',*,*,#3591,.F.);
#4589=ORIENTED_EDGE('',*,*,#3590,.T.);
#4590=ORIENTED_EDGE('',*,*,#3593,.F.);
#4591=ORIENTED_EDGE('',*,*,#3594,.T.);
#4592=ORIENTED_EDGE('',*,*,#3595,.F.);
#4593=ORIENTED_EDGE('',*,*,#3594,.F.);
#4594=ORIENTED_EDGE('',*,*,#3593,.T.);
#4595=ORIENTED_EDGE('',*,*,#3596,.F.);
#4596=ORIENTED_EDGE('',*,*,#3597,.T.);
#4597=ORIENTED_EDGE('',*,*,#3598,.F.);
#4598=ORIENTED_EDGE('',*,*,#3597,.F.);
#4599=ORIENTED_EDGE('',*,*,#3596,.T.);
#4600=ORIENTED_EDGE('',*,*,#3599,.F.);
#4601=ORIENTED_EDGE('',*,*,#3600,.F.);
#4602=ORIENTED_EDGE('',*,*,#3601,.T.);
#4603=ORIENTED_EDGE('',*,*,#3599,.T.);
#4604=ORIENTED_EDGE('',*,*,#3601,.F.);
#4605=ORIENTED_EDGE('',*,*,#3602,.F.);
#4606=ORIENTED_EDGE('',*,*,#3603,.T.);
#4607=ORIENTED_EDGE('',*,*,#3604,.F.);
#4608=ORIENTED_EDGE('',*,*,#3603,.F.);
#4609=ORIENTED_EDGE('',*,*,#3602,.T.);
#4610=ORIENTED_EDGE('',*,*,#3605,.F.);
#4611=ORIENTED_EDGE('',*,*,#3606,.F.);
#4612=ORIENTED_EDGE('',*,*,#3607,.T.);
#4613=ORIENTED_EDGE('',*,*,#3605,.T.);
#4614=ORIENTED_EDGE('',*,*,#3607,.F.);
#4615=ORIENTED_EDGE('',*,*,#3608,.F.);
#4616=ORIENTED_EDGE('',*,*,#3609,.T.);
#4617=ORIENTED_EDGE('',*,*,#3610,.F.);
#4618=ORIENTED_EDGE('',*,*,#3609,.F.);
#4619=ORIENTED_EDGE('',*,*,#3608,.T.);
#4620=ORIENTED_EDGE('',*,*,#3611,.F.);
#4621=ORIENTED_EDGE('',*,*,#3612,.F.);
#4622=ORIENTED_EDGE('',*,*,#3613,.T.);
#4623=ORIENTED_EDGE('',*,*,#3611,.T.);
#4624=ORIENTED_EDGE('',*,*,#3613,.F.);
#4625=ORIENTED_EDGE('',*,*,#3614,.F.);
#4626=ORIENTED_EDGE('',*,*,#3615,.T.);
#4627=ORIENTED_EDGE('',*,*,#3616,.F.);
#4628=ORIENTED_EDGE('',*,*,#3617,.F.);
#4629=ORIENTED_EDGE('',*,*,#3618,.F.);
#4630=ORIENTED_EDGE('',*,*,#3619,.F.);
#4631=ORIENTED_EDGE('',*,*,#3620,.F.);
#4632=ORIENTED_EDGE('',*,*,#3621,.F.);
#4633=ORIENTED_EDGE('',*,*,#3622,.F.);
#4634=ORIENTED_EDGE('',*,*,#3623,.T.);
#4635=ORIENTED_EDGE('',*,*,#3624,.F.);
#4636=ORIENTED_EDGE('',*,*,#3625,.F.);
#4637=ORIENTED_EDGE('',*,*,#3600,.T.);
#4638=ORIENTED_EDGE('',*,*,#3626,.T.);
#4639=ORIENTED_EDGE('',*,*,#3627,.T.);
#4640=ORIENTED_EDGE('',*,*,#3616,.T.);
#4641=ORIENTED_EDGE('',*,*,#3628,.T.);
#4642=ORIENTED_EDGE('',*,*,#3629,.T.);
#4643=ORIENTED_EDGE('',*,*,#3630,.T.);
#4644=ORIENTED_EDGE('',*,*,#3622,.T.);
#4645=ORIENTED_EDGE('',*,*,#3631,.T.);
#4646=ORIENTED_EDGE('',*,*,#3619,.T.);
#4647=ORIENTED_EDGE('',*,*,#3632,.F.);
#4648=ORIENTED_EDGE('',*,*,#3633,.F.);
#4649=ORIENTED_EDGE('',*,*,#3634,.F.);
#4650=ORIENTED_EDGE('',*,*,#3618,.T.);
#4651=ORIENTED_EDGE('',*,*,#3635,.T.);
#4652=ORIENTED_EDGE('',*,*,#3636,.T.);
#4653=ORIENTED_EDGE('',*,*,#3632,.T.);
#4654=ORIENTED_EDGE('',*,*,#3637,.F.);
#4655=ORIENTED_EDGE('',*,*,#3633,.T.);
#4656=ORIENTED_EDGE('',*,*,#3636,.F.);
#4657=ORIENTED_EDGE('',*,*,#3638,.F.);
#4658=ORIENTED_EDGE('',*,*,#3606,.T.);
#4659=ORIENTED_EDGE('',*,*,#3639,.F.);
#4660=ORIENTED_EDGE('',*,*,#3638,.T.);
#4661=ORIENTED_EDGE('',*,*,#3635,.F.);
#4662=ORIENTED_EDGE('',*,*,#3617,.T.);
#4663=ORIENTED_EDGE('',*,*,#3627,.F.);
#4664=ORIENTED_EDGE('',*,*,#3640,.F.);
#4665=ORIENTED_EDGE('',*,*,#3631,.F.);
#4666=ORIENTED_EDGE('',*,*,#3621,.T.);
#4667=ORIENTED_EDGE('',*,*,#3620,.T.);
#4668=ORIENTED_EDGE('',*,*,#3634,.T.);
#4669=ORIENTED_EDGE('',*,*,#3637,.T.);
#4670=ORIENTED_EDGE('',*,*,#3639,.T.);
#4671=ORIENTED_EDGE('',*,*,#3625,.T.);
#4672=ORIENTED_EDGE('',*,*,#3641,.F.);
#4673=ORIENTED_EDGE('',*,*,#3642,.T.);
#4674=ORIENTED_EDGE('',*,*,#3643,.T.);
#4675=ORIENTED_EDGE('',*,*,#3624,.T.);
#4676=ORIENTED_EDGE('',*,*,#3644,.F.);
#4677=ORIENTED_EDGE('',*,*,#3645,.T.);
#4678=ORIENTED_EDGE('',*,*,#3641,.T.);
#4679=ORIENTED_EDGE('',*,*,#3614,.T.);
#4680=ORIENTED_EDGE('',*,*,#3643,.F.);
#4681=ORIENTED_EDGE('',*,*,#3646,.T.);
#4682=ORIENTED_EDGE('',*,*,#3647,.T.);
#4683=ORIENTED_EDGE('',*,*,#3647,.F.);
#4684=ORIENTED_EDGE('',*,*,#3648,.T.);
#4685=ORIENTED_EDGE('',*,*,#3644,.T.);
#4686=ORIENTED_EDGE('',*,*,#3623,.F.);
#4687=ORIENTED_EDGE('',*,*,#3630,.F.);
#4688=ORIENTED_EDGE('',*,*,#3649,.T.);
#4689=ORIENTED_EDGE('',*,*,#3628,.F.);
#4690=ORIENTED_EDGE('',*,*,#3615,.F.);
#4691=ORIENTED_EDGE('',*,*,#3649,.F.);
#4692=ORIENTED_EDGE('',*,*,#3629,.F.);
#4693=ORIENTED_EDGE('',*,*,#3640,.T.);
#4694=ORIENTED_EDGE('',*,*,#3626,.F.);
#4695=ORIENTED_EDGE('',*,*,#3610,.T.);
#4696=ORIENTED_EDGE('',*,*,#3604,.T.);
#4697=ORIENTED_EDGE('',*,*,#3598,.T.);
#4698=ORIENTED_EDGE('',*,*,#3595,.T.);
#4699=ORIENTED_EDGE('',*,*,#3592,.T.);
#4700=ORIENTED_EDGE('',*,*,#3589,.T.);
#4701=ORIENTED_EDGE('',*,*,#3586,.T.);
#4702=ORIENTED_EDGE('',*,*,#3648,.F.);
#4703=ORIENTED_EDGE('',*,*,#3646,.F.);
#4704=ORIENTED_EDGE('',*,*,#3642,.F.);
#4705=ORIENTED_EDGE('',*,*,#3645,.F.);
#4706=ORIENTED_EDGE('',*,*,#3612,.T.);
#4707=ORIENTED_EDGE('',*,*,#3650,.F.);
#4708=ORIENTED_EDGE('',*,*,#3651,.T.);
#4709=ORIENTED_EDGE('',*,*,#3652,.F.);
#4710=ORIENTED_EDGE('',*,*,#3651,.F.);
#4711=ORIENTED_EDGE('',*,*,#3653,.F.);
#4712=ORIENTED_EDGE('',*,*,#3654,.T.);
#4713=ORIENTED_EDGE('',*,*,#3655,.F.);
#4714=ORIENTED_EDGE('',*,*,#3654,.F.);
#4715=ORIENTED_EDGE('',*,*,#3656,.F.);
#4716=ORIENTED_EDGE('',*,*,#3657,.T.);
#4717=ORIENTED_EDGE('',*,*,#3658,.F.);
#4718=ORIENTED_EDGE('',*,*,#3657,.F.);
#4719=ORIENTED_EDGE('',*,*,#3659,.F.);
#4720=ORIENTED_EDGE('',*,*,#3660,.T.);
#4721=ORIENTED_EDGE('',*,*,#3661,.F.);
#4722=ORIENTED_EDGE('',*,*,#3660,.F.);
#4723=ORIENTED_EDGE('',*,*,#3662,.F.);
#4724=ORIENTED_EDGE('',*,*,#3663,.T.);
#4725=ORIENTED_EDGE('',*,*,#3664,.T.);
#4726=ORIENTED_EDGE('',*,*,#3663,.F.);
#4727=ORIENTED_EDGE('',*,*,#3664,.F.);
#4728=ORIENTED_EDGE('',*,*,#3665,.F.);
#4729=ORIENTED_EDGE('',*,*,#3666,.F.);
#4730=ORIENTED_EDGE('',*,*,#3667,.T.);
#4731=ORIENTED_EDGE('',*,*,#3665,.T.);
#4732=ORIENTED_EDGE('',*,*,#3667,.F.);
#4733=ORIENTED_EDGE('',*,*,#3668,.F.);
#4734=ORIENTED_EDGE('',*,*,#3669,.T.);
#4735=ORIENTED_EDGE('',*,*,#3670,.T.);
#4736=ORIENTED_EDGE('',*,*,#3669,.F.);
#4737=ORIENTED_EDGE('',*,*,#3668,.T.);
#4738=ORIENTED_EDGE('',*,*,#3666,.T.);
#4739=ORIENTED_EDGE('',*,*,#3661,.T.);
#4740=ORIENTED_EDGE('',*,*,#3658,.T.);
#4741=ORIENTED_EDGE('',*,*,#3655,.T.);
#4742=ORIENTED_EDGE('',*,*,#3652,.T.);
#4743=ORIENTED_EDGE('',*,*,#3670,.F.);
#4744=ORIENTED_EDGE('',*,*,#3662,.T.);
#4745=ORIENTED_EDGE('',*,*,#3659,.T.);
#4746=ORIENTED_EDGE('',*,*,#3656,.T.);
#4747=ORIENTED_EDGE('',*,*,#3653,.T.);
#4748=ORIENTED_EDGE('',*,*,#3650,.T.);
#4749=ORIENTED_EDGE('',*,*,#3671,.T.);
#4750=ORIENTED_EDGE('',*,*,#3672,.T.);
#4751=ORIENTED_EDGE('',*,*,#3673,.F.);
#4752=ORIENTED_EDGE('',*,*,#3672,.F.);
#4753=ORIENTED_EDGE('',*,*,#3673,.T.);
#4754=ORIENTED_EDGE('',*,*,#3671,.F.);
#4755=ORIENTED_EDGE('',*,*,#3674,.F.);
#4756=ORIENTED_EDGE('',*,*,#3675,.F.);
#4757=ORIENTED_EDGE('',*,*,#3676,.T.);
#4758=ORIENTED_EDGE('',*,*,#3677,.F.);
#4759=ORIENTED_EDGE('',*,*,#3678,.F.);
#4760=ORIENTED_EDGE('',*,*,#3676,.F.);
#4761=ORIENTED_EDGE('',*,*,#3677,.T.);
#4762=ORIENTED_EDGE('',*,*,#3678,.T.);
#4763=ORIENTED_EDGE('',*,*,#3679,.T.);
#4764=ORIENTED_EDGE('',*,*,#3680,.T.);
#4765=ORIENTED_EDGE('',*,*,#3679,.F.);
#4766=ORIENTED_EDGE('',*,*,#3681,.T.);
#4767=ORIENTED_EDGE('',*,*,#3682,.T.);
#4768=ORIENTED_EDGE('',*,*,#3683,.F.);
#4769=ORIENTED_EDGE('',*,*,#3682,.F.);
#4770=ORIENTED_EDGE('',*,*,#3683,.T.);
#4771=ORIENTED_EDGE('',*,*,#3684,.T.);
#4772=ORIENTED_EDGE('',*,*,#3685,.F.);
#4773=ORIENTED_EDGE('',*,*,#3684,.F.);
#4774=ORIENTED_EDGE('',*,*,#3680,.F.);
#4775=ORIENTED_EDGE('',*,*,#3685,.T.);
#4776=ORIENTED_EDGE('',*,*,#3686,.F.);
#4777=ORIENTED_EDGE('',*,*,#3687,.T.);
#4778=ORIENTED_EDGE('',*,*,#3674,.T.);
#4779=ORIENTED_EDGE('',*,*,#3675,.T.);
#4780=ORIENTED_EDGE('',*,*,#3687,.F.);
#4781=ORIENTED_EDGE('',*,*,#3686,.T.);
#4782=ORIENTED_EDGE('',*,*,#3688,.F.);
#4783=ORIENTED_EDGE('',*,*,#3688,.T.);
#4784=ORIENTED_EDGE('',*,*,#3689,.T.);
#4785=ORIENTED_EDGE('',*,*,#3681,.F.);
#4786=ORIENTED_EDGE('',*,*,#3689,.F.);
#4787=ORIENTED_EDGE('',*,*,#3690,.F.);
#4788=ORIENTED_EDGE('',*,*,#3691,.F.);
#4789=ORIENTED_EDGE('',*,*,#3692,.T.);
#4790=ORIENTED_EDGE('',*,*,#3693,.F.);
#4791=ORIENTED_EDGE('',*,*,#3694,.F.);
#4792=ORIENTED_EDGE('',*,*,#3692,.F.);
#4793=ORIENTED_EDGE('',*,*,#3695,.T.);
#4794=ORIENTED_EDGE('',*,*,#3696,.T.);
#4795=ORIENTED_EDGE('',*,*,#3693,.T.);
#4796=ORIENTED_EDGE('',*,*,#3694,.T.);
#4797=ORIENTED_EDGE('',*,*,#3696,.F.);
#4798=ORIENTED_EDGE('',*,*,#3697,.F.);
#4799=ORIENTED_EDGE('',*,*,#3698,.T.);
#4800=ORIENTED_EDGE('',*,*,#3699,.F.);
#4801=ORIENTED_EDGE('',*,*,#3700,.T.);
#4802=ORIENTED_EDGE('',*,*,#3697,.T.);
#4803=ORIENTED_EDGE('',*,*,#3700,.F.);
#4804=ORIENTED_EDGE('',*,*,#3701,.F.);
#4805=ORIENTED_EDGE('',*,*,#3702,.T.);
#4806=ORIENTED_EDGE('',*,*,#3699,.T.);
#4807=ORIENTED_EDGE('',*,*,#3702,.F.);
#4808=ORIENTED_EDGE('',*,*,#3703,.F.);
#4809=ORIENTED_EDGE('',*,*,#3704,.T.);
#4810=ORIENTED_EDGE('',*,*,#3701,.T.);
#4811=ORIENTED_EDGE('',*,*,#3704,.F.);
#4812=ORIENTED_EDGE('',*,*,#3703,.T.);
#4813=ORIENTED_EDGE('',*,*,#3695,.F.);
#4814=ORIENTED_EDGE('',*,*,#3690,.T.);
#4815=ORIENTED_EDGE('',*,*,#3691,.T.);
#4816=ORIENTED_EDGE('',*,*,#3705,.T.);
#4817=ORIENTED_EDGE('',*,*,#3698,.F.);
#4818=ORIENTED_EDGE('',*,*,#3705,.F.);
#4819=ORIENTED_EDGE('',*,*,#3706,.T.);
#4820=ORIENTED_EDGE('',*,*,#3706,.F.);
#4821=ORIENTED_EDGE('',*,*,#3707,.T.);
#4822=ORIENTED_EDGE('',*,*,#3707,.F.);
#4823=ORIENTED_EDGE('',*,*,#3708,.T.);
#4824=ORIENTED_EDGE('',*,*,#3708,.F.);
#4825=ORIENTED_EDGE('',*,*,#3709,.T.);
#4826=ORIENTED_EDGE('',*,*,#3709,.F.);
#4827=ORIENTED_EDGE('',*,*,#3710,.T.);
#4828=ORIENTED_EDGE('',*,*,#3710,.F.);
#4829=ORIENTED_EDGE('',*,*,#3711,.T.);
#4830=ORIENTED_EDGE('',*,*,#3711,.F.);
#4831=ORIENTED_EDGE('',*,*,#3712,.T.);
#4832=ORIENTED_EDGE('',*,*,#3712,.F.);
#4833=ORIENTED_EDGE('',*,*,#3713,.F.);
#4834=ORIENTED_EDGE('',*,*,#3714,.F.);
#4835=ORIENTED_EDGE('',*,*,#3715,.F.);
#4836=ORIENTED_EDGE('',*,*,#3716,.F.);
#4837=ORIENTED_EDGE('',*,*,#3715,.T.);
#4838=ORIENTED_EDGE('',*,*,#3717,.F.);
#4839=ORIENTED_EDGE('',*,*,#3718,.T.);
#4840=ORIENTED_EDGE('',*,*,#3719,.F.);
#4841=ORIENTED_EDGE('',*,*,#3720,.T.);
#4842=ORIENTED_EDGE('',*,*,#3721,.F.);
#4843=ORIENTED_EDGE('',*,*,#3722,.T.);
#4844=ORIENTED_EDGE('',*,*,#3723,.F.);
#4845=ORIENTED_EDGE('',*,*,#3722,.F.);
#4846=ORIENTED_EDGE('',*,*,#3724,.F.);
#4847=ORIENTED_EDGE('',*,*,#3725,.T.);
#4848=ORIENTED_EDGE('',*,*,#3726,.F.);
#4849=ORIENTED_EDGE('',*,*,#3727,.T.);
#4850=ORIENTED_EDGE('',*,*,#3728,.F.);
#4851=ORIENTED_EDGE('',*,*,#3729,.T.);
#4852=ORIENTED_EDGE('',*,*,#3730,.F.);
#4853=ORIENTED_EDGE('',*,*,#3731,.T.);
#4854=ORIENTED_EDGE('',*,*,#3732,.F.);
#4855=ORIENTED_EDGE('',*,*,#3714,.T.);
#4856=ORIENTED_EDGE('',*,*,#3733,.T.);
#4857=ORIENTED_EDGE('',*,*,#3734,.T.);
#4858=ORIENTED_EDGE('',*,*,#3717,.T.);
#4859=ORIENTED_EDGE('',*,*,#3735,.F.);
#4860=ORIENTED_EDGE('',*,*,#3736,.F.);
#4861=ORIENTED_EDGE('',*,*,#3718,.F.);
#4862=ORIENTED_EDGE('',*,*,#3734,.F.);
#4863=ORIENTED_EDGE('',*,*,#3736,.T.);
#4864=ORIENTED_EDGE('',*,*,#3737,.T.);
#4865=ORIENTED_EDGE('',*,*,#3738,.T.);
#4866=ORIENTED_EDGE('',*,*,#3719,.T.);
#4867=ORIENTED_EDGE('',*,*,#3739,.F.);
#4868=ORIENTED_EDGE('',*,*,#3740,.F.);
#4869=ORIENTED_EDGE('',*,*,#3720,.F.);
#4870=ORIENTED_EDGE('',*,*,#3738,.F.);
#4871=ORIENTED_EDGE('',*,*,#3740,.T.);
#4872=ORIENTED_EDGE('',*,*,#3741,.T.);
#4873=ORIENTED_EDGE('',*,*,#3742,.T.);
#4874=ORIENTED_EDGE('',*,*,#3743,.T.);
#4875=ORIENTED_EDGE('',*,*,#3724,.T.);
#4876=ORIENTED_EDGE('',*,*,#3721,.T.);
#4877=ORIENTED_EDGE('',*,*,#3744,.F.);
#4878=ORIENTED_EDGE('',*,*,#3745,.F.);
#4879=ORIENTED_EDGE('',*,*,#3725,.F.);
#4880=ORIENTED_EDGE('',*,*,#3743,.F.);
#4881=ORIENTED_EDGE('',*,*,#3745,.T.);
#4882=ORIENTED_EDGE('',*,*,#3746,.T.);
#4883=ORIENTED_EDGE('',*,*,#3747,.T.);
#4884=ORIENTED_EDGE('',*,*,#3726,.T.);
#4885=ORIENTED_EDGE('',*,*,#3748,.F.);
#4886=ORIENTED_EDGE('',*,*,#3749,.F.);
#4887=ORIENTED_EDGE('',*,*,#3727,.F.);
#4888=ORIENTED_EDGE('',*,*,#3747,.F.);
#4889=ORIENTED_EDGE('',*,*,#3749,.T.);
#4890=ORIENTED_EDGE('',*,*,#3750,.T.);
#4891=ORIENTED_EDGE('',*,*,#3751,.T.);
#4892=ORIENTED_EDGE('',*,*,#3728,.T.);
#4893=ORIENTED_EDGE('',*,*,#3729,.F.);
#4894=ORIENTED_EDGE('',*,*,#3751,.F.);
#4895=ORIENTED_EDGE('',*,*,#3752,.F.);
#4896=ORIENTED_EDGE('',*,*,#3753,.F.);
#4897=ORIENTED_EDGE('',*,*,#3754,.F.);
#4898=ORIENTED_EDGE('',*,*,#3755,.T.);
#4899=ORIENTED_EDGE('',*,*,#3741,.F.);
#4900=ORIENTED_EDGE('',*,*,#3739,.T.);
#4901=ORIENTED_EDGE('',*,*,#3737,.F.);
#4902=ORIENTED_EDGE('',*,*,#3735,.T.);
#4903=ORIENTED_EDGE('',*,*,#3733,.F.);
#4904=ORIENTED_EDGE('',*,*,#3713,.T.);
#4905=ORIENTED_EDGE('',*,*,#3756,.F.);
#4906=ORIENTED_EDGE('',*,*,#3757,.T.);
#4907=ORIENTED_EDGE('',*,*,#3758,.F.);
#4908=ORIENTED_EDGE('',*,*,#3752,.T.);
#4909=ORIENTED_EDGE('',*,*,#3750,.F.);
#4910=ORIENTED_EDGE('',*,*,#3748,.T.);
#4911=ORIENTED_EDGE('',*,*,#3746,.F.);
#4912=ORIENTED_EDGE('',*,*,#3744,.T.);
#4913=ORIENTED_EDGE('',*,*,#3742,.F.);
#4914=ORIENTED_EDGE('',*,*,#3755,.F.);
#4915=ORIENTED_EDGE('',*,*,#3716,.T.);
#4916=ORIENTED_EDGE('',*,*,#3732,.T.);
#4917=ORIENTED_EDGE('',*,*,#3759,.T.);
#4918=ORIENTED_EDGE('',*,*,#3756,.T.);
#4919=ORIENTED_EDGE('',*,*,#3731,.F.);
#4920=ORIENTED_EDGE('',*,*,#3760,.F.);
#4921=ORIENTED_EDGE('',*,*,#3757,.F.);
#4922=ORIENTED_EDGE('',*,*,#3759,.F.);
#4923=ORIENTED_EDGE('',*,*,#3723,.T.);
#4924=ORIENTED_EDGE('',*,*,#3754,.T.);
#4925=ORIENTED_EDGE('',*,*,#3753,.T.);
#4926=ORIENTED_EDGE('',*,*,#3758,.T.);
#4927=ORIENTED_EDGE('',*,*,#3760,.T.);
#4928=ORIENTED_EDGE('',*,*,#3730,.T.);
#4929=ORIENTED_EDGE('',*,*,#3761,.F.);
#4930=ORIENTED_EDGE('',*,*,#3762,.T.);
#4931=ORIENTED_EDGE('',*,*,#3763,.F.);
#4932=ORIENTED_EDGE('',*,*,#3764,.T.);
#4933=ORIENTED_EDGE('',*,*,#3761,.T.);
#4934=ORIENTED_EDGE('',*,*,#3764,.F.);
#4935=ORIENTED_EDGE('',*,*,#3763,.T.);
#4936=ORIENTED_EDGE('',*,*,#3765,.F.);
#4937=ORIENTED_EDGE('',*,*,#3765,.T.);
#4938=ORIENTED_EDGE('',*,*,#3766,.T.);
#4939=ORIENTED_EDGE('',*,*,#3762,.F.);
#4940=ORIENTED_EDGE('',*,*,#3766,.F.);
#4941=ORIENTED_EDGE('',*,*,#3767,.F.);
#4942=ORIENTED_EDGE('',*,*,#3768,.T.);
#4943=ORIENTED_EDGE('',*,*,#3769,.F.);
#4944=ORIENTED_EDGE('',*,*,#3770,.T.);
#4945=ORIENTED_EDGE('',*,*,#3767,.T.);
#4946=ORIENTED_EDGE('',*,*,#3770,.F.);
#4947=ORIENTED_EDGE('',*,*,#3769,.T.);
#4948=ORIENTED_EDGE('',*,*,#3771,.F.);
#4949=ORIENTED_EDGE('',*,*,#3771,.T.);
#4950=ORIENTED_EDGE('',*,*,#3772,.T.);
#4951=ORIENTED_EDGE('',*,*,#3768,.F.);
#4952=ORIENTED_EDGE('',*,*,#3772,.F.);
#4953=ORIENTED_EDGE('',*,*,#3773,.F.);
#4954=ORIENTED_EDGE('',*,*,#3774,.F.);
#4955=ORIENTED_EDGE('',*,*,#3775,.T.);
#4956=ORIENTED_EDGE('',*,*,#3773,.T.);
#4957=ORIENTED_EDGE('',*,*,#3775,.F.);
#4958=ORIENTED_EDGE('',*,*,#3776,.F.);
#4959=ORIENTED_EDGE('',*,*,#3777,.T.);
#4960=ORIENTED_EDGE('',*,*,#3774,.T.);
#4961=ORIENTED_EDGE('',*,*,#3777,.F.);
#4962=ORIENTED_EDGE('',*,*,#3778,.F.);
#4963=ORIENTED_EDGE('',*,*,#3779,.T.);
#4964=ORIENTED_EDGE('',*,*,#3776,.T.);
#4965=ORIENTED_EDGE('',*,*,#3779,.F.);
#4966=ORIENTED_EDGE('',*,*,#3778,.T.);
#4967=ORIENTED_EDGE('',*,*,#3780,.F.);
#4968=ORIENTED_EDGE('',*,*,#3781,.F.);
#4969=ORIENTED_EDGE('',*,*,#3782,.T.);
#4970=ORIENTED_EDGE('',*,*,#3780,.T.);
#4971=ORIENTED_EDGE('',*,*,#3782,.F.);
#4972=ORIENTED_EDGE('',*,*,#3783,.F.);
#4973=ORIENTED_EDGE('',*,*,#3784,.T.);
#4974=ORIENTED_EDGE('',*,*,#3781,.T.);
#4975=ORIENTED_EDGE('',*,*,#3784,.F.);
#4976=ORIENTED_EDGE('',*,*,#3785,.F.);
#4977=ORIENTED_EDGE('',*,*,#3786,.T.);
#4978=ORIENTED_EDGE('',*,*,#3783,.T.);
#4979=ORIENTED_EDGE('',*,*,#3786,.F.);
#4980=ORIENTED_EDGE('',*,*,#3785,.T.);
#4981=ORIENTED_EDGE('',*,*,#3787,.T.);
#4982=ORIENTED_EDGE('',*,*,#3788,.T.);
#4983=ORIENTED_EDGE('',*,*,#3789,.T.);
#4984=ORIENTED_EDGE('',*,*,#3790,.F.);
#4985=ORIENTED_EDGE('',*,*,#3791,.T.);
#4986=ORIENTED_EDGE('',*,*,#3792,.T.);
#4987=ORIENTED_EDGE('',*,*,#3793,.T.);
#4988=ORIENTED_EDGE('',*,*,#3788,.F.);
#4989=ORIENTED_EDGE('',*,*,#3794,.T.);
#4990=ORIENTED_EDGE('',*,*,#3795,.T.);
#4991=ORIENTED_EDGE('',*,*,#3796,.T.);
#4992=ORIENTED_EDGE('',*,*,#3792,.F.);
#4993=ORIENTED_EDGE('',*,*,#3797,.T.);
#4994=ORIENTED_EDGE('',*,*,#3798,.T.);
#4995=ORIENTED_EDGE('',*,*,#3799,.T.);
#4996=ORIENTED_EDGE('',*,*,#3795,.F.);
#4997=ORIENTED_EDGE('',*,*,#3800,.T.);
#4998=ORIENTED_EDGE('',*,*,#3801,.T.);
#4999=ORIENTED_EDGE('',*,*,#3802,.T.);
#5000=ORIENTED_EDGE('',*,*,#3798,.F.);
#5001=ORIENTED_EDGE('',*,*,#3803,.T.);
#5002=ORIENTED_EDGE('',*,*,#3790,.T.);
#5003=ORIENTED_EDGE('',*,*,#3804,.T.);
#5004=ORIENTED_EDGE('',*,*,#3801,.F.);
#5005=ORIENTED_EDGE('',*,*,#3803,.F.);
#5006=ORIENTED_EDGE('',*,*,#3800,.F.);
#5007=ORIENTED_EDGE('',*,*,#3797,.F.);
#5008=ORIENTED_EDGE('',*,*,#3794,.F.);
#5009=ORIENTED_EDGE('',*,*,#3791,.F.);
#5010=ORIENTED_EDGE('',*,*,#3787,.F.);
#5011=ORIENTED_EDGE('',*,*,#3804,.F.);
#5012=ORIENTED_EDGE('',*,*,#3789,.F.);
#5013=ORIENTED_EDGE('',*,*,#3793,.F.);
#5014=ORIENTED_EDGE('',*,*,#3796,.F.);
#5015=ORIENTED_EDGE('',*,*,#3799,.F.);
#5016=ORIENTED_EDGE('',*,*,#3802,.F.);
#5017=ORIENTED_EDGE('',*,*,#3805,.F.);
#5018=ORIENTED_EDGE('',*,*,#3806,.F.);
#5019=ORIENTED_EDGE('',*,*,#3807,.F.);
#5020=ORIENTED_EDGE('',*,*,#3808,.F.);
#5021=ORIENTED_EDGE('',*,*,#3809,.F.);
#5022=ORIENTED_EDGE('',*,*,#3808,.T.);
#5023=ORIENTED_EDGE('',*,*,#3810,.F.);
#5024=ORIENTED_EDGE('',*,*,#3811,.T.);
#5025=ORIENTED_EDGE('',*,*,#3812,.F.);
#5026=ORIENTED_EDGE('',*,*,#3811,.F.);
#5027=ORIENTED_EDGE('',*,*,#3813,.F.);
#5028=ORIENTED_EDGE('',*,*,#3814,.F.);
#5029=ORIENTED_EDGE('',*,*,#3815,.F.);
#5030=ORIENTED_EDGE('',*,*,#3814,.T.);
#5031=ORIENTED_EDGE('',*,*,#3816,.T.);
#5032=ORIENTED_EDGE('',*,*,#3806,.T.);
#5033=ORIENTED_EDGE('',*,*,#3816,.F.);
#5034=ORIENTED_EDGE('',*,*,#3813,.T.);
#5035=ORIENTED_EDGE('',*,*,#3810,.T.);
#5036=ORIENTED_EDGE('',*,*,#3807,.T.);
#5037=ORIENTED_EDGE('',*,*,#3817,.F.);
#5038=ORIENTED_EDGE('',*,*,#3818,.T.);
#5039=ORIENTED_EDGE('',*,*,#3819,.F.);
#5040=ORIENTED_EDGE('',*,*,#3820,.T.);
#5041=ORIENTED_EDGE('',*,*,#3817,.T.);
#5042=ORIENTED_EDGE('',*,*,#3820,.F.);
#5043=ORIENTED_EDGE('',*,*,#3819,.T.);
#5044=ORIENTED_EDGE('',*,*,#3821,.F.);
#5045=ORIENTED_EDGE('',*,*,#3822,.F.);
#5046=ORIENTED_EDGE('',*,*,#3823,.T.);
#5047=ORIENTED_EDGE('',*,*,#3821,.T.);
#5048=ORIENTED_EDGE('',*,*,#3823,.F.);
#5049=ORIENTED_EDGE('',*,*,#3824,.F.);
#5050=ORIENTED_EDGE('',*,*,#3822,.T.);
#5051=ORIENTED_EDGE('',*,*,#3825,.F.);
#5052=ORIENTED_EDGE('',*,*,#3826,.T.);
#5053=ORIENTED_EDGE('',*,*,#3824,.T.);
#5054=ORIENTED_EDGE('',*,*,#3826,.F.);
#5055=ORIENTED_EDGE('',*,*,#3825,.T.);
#5056=ORIENTED_EDGE('',*,*,#3827,.F.);
#5057=ORIENTED_EDGE('',*,*,#3828,.F.);
#5058=ORIENTED_EDGE('',*,*,#3829,.T.);
#5059=ORIENTED_EDGE('',*,*,#3827,.T.);
#5060=ORIENTED_EDGE('',*,*,#3829,.F.);
#5061=ORIENTED_EDGE('',*,*,#3830,.F.);
#5062=ORIENTED_EDGE('',*,*,#3828,.T.);
#5063=ORIENTED_EDGE('',*,*,#3831,.F.);
#5064=ORIENTED_EDGE('',*,*,#3832,.T.);
#5065=ORIENTED_EDGE('',*,*,#3830,.T.);
#5066=ORIENTED_EDGE('',*,*,#3832,.F.);
#5067=ORIENTED_EDGE('',*,*,#3831,.T.);
#5068=ORIENTED_EDGE('',*,*,#3833,.F.);
#5069=ORIENTED_EDGE('',*,*,#3833,.T.);
#5070=ORIENTED_EDGE('',*,*,#3834,.T.);
#5071=ORIENTED_EDGE('',*,*,#3818,.F.);
#5072=ORIENTED_EDGE('',*,*,#3834,.F.);
#5073=ORIENTED_EDGE('',*,*,#3812,.T.);
#5074=ORIENTED_EDGE('',*,*,#3815,.T.);
#5075=ORIENTED_EDGE('',*,*,#3805,.T.);
#5076=ORIENTED_EDGE('',*,*,#3809,.T.);
#5077=ORIENTED_EDGE('',*,*,#3835,.F.);
#5078=ORIENTED_EDGE('',*,*,#3836,.F.);
#5079=ORIENTED_EDGE('',*,*,#3837,.F.);
#5080=ORIENTED_EDGE('',*,*,#3838,.F.);
#5081=ORIENTED_EDGE('',*,*,#3839,.F.);
#5082=ORIENTED_EDGE('',*,*,#3838,.T.);
#5083=ORIENTED_EDGE('',*,*,#3840,.F.);
#5084=ORIENTED_EDGE('',*,*,#3841,.T.);
#5085=ORIENTED_EDGE('',*,*,#3842,.F.);
#5086=ORIENTED_EDGE('',*,*,#3841,.F.);
#5087=ORIENTED_EDGE('',*,*,#3843,.F.);
#5088=ORIENTED_EDGE('',*,*,#3844,.F.);
#5089=ORIENTED_EDGE('',*,*,#3845,.F.);
#5090=ORIENTED_EDGE('',*,*,#3844,.T.);
#5091=ORIENTED_EDGE('',*,*,#3846,.F.);
#5092=ORIENTED_EDGE('',*,*,#3836,.T.);
#5093=ORIENTED_EDGE('',*,*,#3847,.F.);
#5094=ORIENTED_EDGE('',*,*,#3848,.T.);
#5095=ORIENTED_EDGE('',*,*,#3849,.F.);
#5096=ORIENTED_EDGE('',*,*,#3850,.T.);
#5097=ORIENTED_EDGE('',*,*,#3847,.T.);
#5098=ORIENTED_EDGE('',*,*,#3850,.F.);
#5099=ORIENTED_EDGE('',*,*,#3842,.T.);
#5100=ORIENTED_EDGE('',*,*,#3845,.T.);
#5101=ORIENTED_EDGE('',*,*,#3835,.T.);
#5102=ORIENTED_EDGE('',*,*,#3839,.T.);
#5103=ORIENTED_EDGE('',*,*,#3849,.T.);
#5104=ORIENTED_EDGE('',*,*,#3851,.F.);
#5105=ORIENTED_EDGE('',*,*,#3851,.T.);
#5106=ORIENTED_EDGE('',*,*,#3852,.T.);
#5107=ORIENTED_EDGE('',*,*,#3848,.F.);
#5108=ORIENTED_EDGE('',*,*,#3852,.F.);
#5109=ORIENTED_EDGE('',*,*,#3843,.T.);
#5110=ORIENTED_EDGE('',*,*,#3840,.T.);
#5111=ORIENTED_EDGE('',*,*,#3837,.T.);
#5112=ORIENTED_EDGE('',*,*,#3846,.T.);
#5113=ORIENTED_EDGE('',*,*,#3853,.T.);
#5114=ORIENTED_EDGE('',*,*,#3854,.T.);
#5115=ORIENTED_EDGE('',*,*,#3855,.T.);
#5116=ORIENTED_EDGE('',*,*,#3856,.F.);
#5117=ORIENTED_EDGE('',*,*,#3857,.T.);
#5118=ORIENTED_EDGE('',*,*,#3858,.T.);
#5119=ORIENTED_EDGE('',*,*,#3859,.T.);
#5120=ORIENTED_EDGE('',*,*,#3854,.F.);
#5121=ORIENTED_EDGE('',*,*,#3860,.T.);
#5122=ORIENTED_EDGE('',*,*,#3861,.T.);
#5123=ORIENTED_EDGE('',*,*,#3862,.T.);
#5124=ORIENTED_EDGE('',*,*,#3858,.F.);
#5125=ORIENTED_EDGE('',*,*,#3863,.T.);
#5126=ORIENTED_EDGE('',*,*,#3864,.T.);
#5127=ORIENTED_EDGE('',*,*,#3865,.T.);
#5128=ORIENTED_EDGE('',*,*,#3861,.F.);
#5129=ORIENTED_EDGE('',*,*,#3866,.T.);
#5130=ORIENTED_EDGE('',*,*,#3867,.T.);
#5131=ORIENTED_EDGE('',*,*,#3868,.T.);
#5132=ORIENTED_EDGE('',*,*,#3864,.F.);
#5133=ORIENTED_EDGE('',*,*,#3869,.T.);
#5134=ORIENTED_EDGE('',*,*,#3856,.T.);
#5135=ORIENTED_EDGE('',*,*,#3870,.T.);
#5136=ORIENTED_EDGE('',*,*,#3867,.F.);
#5137=ORIENTED_EDGE('',*,*,#3869,.F.);
#5138=ORIENTED_EDGE('',*,*,#3866,.F.);
#5139=ORIENTED_EDGE('',*,*,#3863,.F.);
#5140=ORIENTED_EDGE('',*,*,#3860,.F.);
#5141=ORIENTED_EDGE('',*,*,#3857,.F.);
#5142=ORIENTED_EDGE('',*,*,#3853,.F.);
#5143=ORIENTED_EDGE('',*,*,#3870,.F.);
#5144=ORIENTED_EDGE('',*,*,#3855,.F.);
#5145=ORIENTED_EDGE('',*,*,#3859,.F.);
#5146=ORIENTED_EDGE('',*,*,#3862,.F.);
#5147=ORIENTED_EDGE('',*,*,#3865,.F.);
#5148=ORIENTED_EDGE('',*,*,#3868,.F.);
#5149=ORIENTED_EDGE('',*,*,#3871,.F.);
#5150=ORIENTED_EDGE('',*,*,#3872,.F.);
#5151=ORIENTED_EDGE('',*,*,#3873,.F.);
#5152=ORIENTED_EDGE('',*,*,#3874,.T.);
#5153=ORIENTED_EDGE('',*,*,#3872,.T.);
#5154=ORIENTED_EDGE('',*,*,#3874,.F.);
#5155=ORIENTED_EDGE('',*,*,#3875,.F.);
#5156=ORIENTED_EDGE('',*,*,#3876,.T.);
#5157=ORIENTED_EDGE('',*,*,#3873,.T.);
#5158=ORIENTED_EDGE('',*,*,#3876,.F.);
#5159=ORIENTED_EDGE('',*,*,#3877,.F.);
#5160=ORIENTED_EDGE('',*,*,#3878,.T.);
#5161=ORIENTED_EDGE('',*,*,#3875,.T.);
#5162=ORIENTED_EDGE('',*,*,#3878,.F.);
#5163=ORIENTED_EDGE('',*,*,#3877,.T.);
#5164=ORIENTED_EDGE('',*,*,#3879,.F.);
#5165=ORIENTED_EDGE('',*,*,#3880,.F.);
#5166=ORIENTED_EDGE('',*,*,#3881,.T.);
#5167=ORIENTED_EDGE('',*,*,#3879,.T.);
#5168=ORIENTED_EDGE('',*,*,#3881,.F.);
#5169=ORIENTED_EDGE('',*,*,#3871,.T.);
#5170=ORIENTED_EDGE('',*,*,#3882,.T.);
#5171=ORIENTED_EDGE('',*,*,#3880,.T.);
#5172=ORIENTED_EDGE('',*,*,#3882,.F.);
#5173=ORIENTED_EDGE('',*,*,#3883,.F.);
#5174=ORIENTED_EDGE('',*,*,#3884,.T.);
#5175=ORIENTED_EDGE('',*,*,#3885,.F.);
#5176=ORIENTED_EDGE('',*,*,#3884,.F.);
#5177=ORIENTED_EDGE('',*,*,#3883,.T.);
#5178=ORIENTED_EDGE('',*,*,#3886,.F.);
#5179=ORIENTED_EDGE('',*,*,#3887,.T.);
#5180=ORIENTED_EDGE('',*,*,#3888,.T.);
#5181=ORIENTED_EDGE('',*,*,#3887,.F.);
#5182=ORIENTED_EDGE('',*,*,#3888,.F.);
#5183=ORIENTED_EDGE('',*,*,#3889,.F.);
#5184=ORIENTED_EDGE('',*,*,#3890,.T.);
#5185=ORIENTED_EDGE('',*,*,#3891,.F.);
#5186=ORIENTED_EDGE('',*,*,#3892,.T.);
#5187=ORIENTED_EDGE('',*,*,#3893,.F.);
#5188=ORIENTED_EDGE('',*,*,#3892,.F.);
#5189=ORIENTED_EDGE('',*,*,#3894,.F.);
#5190=ORIENTED_EDGE('',*,*,#3895,.F.);
#5191=ORIENTED_EDGE('',*,*,#3896,.F.);
#5192=ORIENTED_EDGE('',*,*,#3895,.T.);
#5193=ORIENTED_EDGE('',*,*,#3897,.T.);
#5194=ORIENTED_EDGE('',*,*,#3898,.T.);
#5195=ORIENTED_EDGE('',*,*,#3894,.T.);
#5196=ORIENTED_EDGE('',*,*,#3891,.T.);
#5197=ORIENTED_EDGE('',*,*,#3899,.T.);
#5198=ORIENTED_EDGE('',*,*,#3897,.F.);
#5199=ORIENTED_EDGE('',*,*,#3900,.F.);
#5200=ORIENTED_EDGE('',*,*,#3898,.F.);
#5201=ORIENTED_EDGE('',*,*,#3899,.F.);
#5202=ORIENTED_EDGE('',*,*,#3890,.F.);
#5203=ORIENTED_EDGE('',*,*,#3901,.F.);
#5204=ORIENTED_EDGE('',*,*,#3902,.T.);
#5205=ORIENTED_EDGE('',*,*,#3903,.F.);
#5206=ORIENTED_EDGE('',*,*,#3904,.T.);
#5207=ORIENTED_EDGE('',*,*,#3905,.F.);
#5208=ORIENTED_EDGE('',*,*,#3904,.F.);
#5209=ORIENTED_EDGE('',*,*,#3906,.F.);
#5210=ORIENTED_EDGE('',*,*,#3907,.F.);
#5211=ORIENTED_EDGE('',*,*,#3908,.F.);
#5212=ORIENTED_EDGE('',*,*,#3907,.T.);
#5213=ORIENTED_EDGE('',*,*,#3909,.T.);
#5214=ORIENTED_EDGE('',*,*,#3910,.T.);
#5215=ORIENTED_EDGE('',*,*,#3906,.T.);
#5216=ORIENTED_EDGE('',*,*,#3903,.T.);
#5217=ORIENTED_EDGE('',*,*,#3911,.T.);
#5218=ORIENTED_EDGE('',*,*,#3909,.F.);
#5219=ORIENTED_EDGE('',*,*,#3912,.F.);
#5220=ORIENTED_EDGE('',*,*,#3910,.F.);
#5221=ORIENTED_EDGE('',*,*,#3911,.F.);
#5222=ORIENTED_EDGE('',*,*,#3902,.F.);
#5223=ORIENTED_EDGE('',*,*,#3913,.F.);
#5224=ORIENTED_EDGE('',*,*,#3914,.T.);
#5225=ORIENTED_EDGE('',*,*,#3915,.T.);
#5226=ORIENTED_EDGE('',*,*,#3914,.F.);
#5227=ORIENTED_EDGE('',*,*,#3896,.T.);
#5228=ORIENTED_EDGE('',*,*,#3900,.T.);
#5229=ORIENTED_EDGE('',*,*,#3889,.T.);
#5230=ORIENTED_EDGE('',*,*,#3893,.T.);
#5231=ORIENTED_EDGE('',*,*,#3908,.T.);
#5232=ORIENTED_EDGE('',*,*,#3912,.T.);
#5233=ORIENTED_EDGE('',*,*,#3901,.T.);
#5234=ORIENTED_EDGE('',*,*,#3905,.T.);
#5235=ORIENTED_EDGE('',*,*,#3913,.T.);
#5236=ORIENTED_EDGE('',*,*,#3885,.T.);
#5237=ORIENTED_EDGE('',*,*,#3915,.F.);
#5238=ORIENTED_EDGE('',*,*,#3886,.T.);
#5239=ORIENTED_EDGE('',*,*,#3916,.F.);
#5240=ORIENTED_EDGE('',*,*,#3917,.T.);
#5241=ORIENTED_EDGE('',*,*,#3918,.T.);
#5242=ORIENTED_EDGE('',*,*,#3917,.F.);
#5243=ORIENTED_EDGE('',*,*,#3919,.F.);
#5244=ORIENTED_EDGE('',*,*,#3920,.T.);
#5245=ORIENTED_EDGE('',*,*,#3921,.T.);
#5246=ORIENTED_EDGE('',*,*,#3920,.F.);
#5247=ORIENTED_EDGE('',*,*,#3919,.T.);
#5248=ORIENTED_EDGE('',*,*,#3916,.T.);
#5249=ORIENTED_EDGE('',*,*,#3921,.F.);
#5250=ORIENTED_EDGE('',*,*,#3918,.F.);
#5251=ORIENTED_EDGE('',*,*,#3922,.F.);
#5252=ORIENTED_EDGE('',*,*,#3923,.T.);
#5253=ORIENTED_EDGE('',*,*,#3924,.T.);
#5254=ORIENTED_EDGE('',*,*,#3923,.F.);
#5255=ORIENTED_EDGE('',*,*,#3925,.F.);
#5256=ORIENTED_EDGE('',*,*,#3926,.T.);
#5257=ORIENTED_EDGE('',*,*,#3927,.T.);
#5258=ORIENTED_EDGE('',*,*,#3926,.F.);
#5259=ORIENTED_EDGE('',*,*,#3925,.T.);
#5260=ORIENTED_EDGE('',*,*,#3922,.T.);
#5261=ORIENTED_EDGE('',*,*,#3927,.F.);
#5262=ORIENTED_EDGE('',*,*,#3924,.F.);
#5263=ORIENTED_EDGE('',*,*,#3928,.F.);
#5264=ORIENTED_EDGE('',*,*,#3929,.T.);
#5265=ORIENTED_EDGE('',*,*,#3930,.T.);
#5266=ORIENTED_EDGE('',*,*,#3929,.F.);
#5267=ORIENTED_EDGE('',*,*,#3931,.F.);
#5268=ORIENTED_EDGE('',*,*,#3932,.T.);
#5269=ORIENTED_EDGE('',*,*,#3933,.T.);
#5270=ORIENTED_EDGE('',*,*,#3932,.F.);
#5271=ORIENTED_EDGE('',*,*,#3931,.T.);
#5272=ORIENTED_EDGE('',*,*,#3928,.T.);
#5273=ORIENTED_EDGE('',*,*,#3933,.F.);
#5274=ORIENTED_EDGE('',*,*,#3930,.F.);
#5275=ORIENTED_EDGE('',*,*,#3934,.F.);
#5276=ORIENTED_EDGE('',*,*,#3935,.T.);
#5277=ORIENTED_EDGE('',*,*,#3936,.T.);
#5278=ORIENTED_EDGE('',*,*,#3935,.F.);
#5279=ORIENTED_EDGE('',*,*,#3937,.F.);
#5280=ORIENTED_EDGE('',*,*,#3938,.T.);
#5281=ORIENTED_EDGE('',*,*,#3939,.T.);
#5282=ORIENTED_EDGE('',*,*,#3938,.F.);
#5283=ORIENTED_EDGE('',*,*,#3937,.T.);
#5284=ORIENTED_EDGE('',*,*,#3934,.T.);
#5285=ORIENTED_EDGE('',*,*,#3939,.F.);
#5286=ORIENTED_EDGE('',*,*,#3936,.F.);
#5287=ORIENTED_EDGE('',*,*,#3940,.F.);
#5288=ORIENTED_EDGE('',*,*,#3941,.T.);
#5289=ORIENTED_EDGE('',*,*,#3942,.F.);
#5290=ORIENTED_EDGE('',*,*,#3943,.F.);
#5291=ORIENTED_EDGE('',*,*,#3944,.F.);
#5292=ORIENTED_EDGE('',*,*,#3945,.T.);
#5293=ORIENTED_EDGE('',*,*,#3946,.F.);
#5294=ORIENTED_EDGE('',*,*,#3941,.F.);
#5295=ORIENTED_EDGE('',*,*,#3947,.F.);
#5296=ORIENTED_EDGE('',*,*,#3948,.F.);
#5297=ORIENTED_EDGE('',*,*,#3949,.F.);
#5298=ORIENTED_EDGE('',*,*,#3945,.F.);
#5299=ORIENTED_EDGE('',*,*,#3950,.T.);
#5300=ORIENTED_EDGE('',*,*,#3942,.T.);
#5301=ORIENTED_EDGE('',*,*,#3946,.T.);
#5302=ORIENTED_EDGE('',*,*,#3949,.T.);
#5303=ORIENTED_EDGE('',*,*,#3951,.T.);
#5304=ORIENTED_EDGE('',*,*,#3943,.T.);
#5305=ORIENTED_EDGE('',*,*,#3951,.F.);
#5306=ORIENTED_EDGE('',*,*,#3948,.T.);
#5307=ORIENTED_EDGE('',*,*,#3952,.F.);
#5308=ORIENTED_EDGE('',*,*,#3953,.F.);
#5309=ORIENTED_EDGE('',*,*,#3954,.T.);
#5310=ORIENTED_EDGE('',*,*,#3955,.T.);
#5311=ORIENTED_EDGE('',*,*,#3954,.F.);
#5312=ORIENTED_EDGE('',*,*,#3950,.F.);
#5313=ORIENTED_EDGE('',*,*,#3956,.T.);
#5314=ORIENTED_EDGE('',*,*,#3957,.F.);
#5315=ORIENTED_EDGE('',*,*,#3956,.F.);
#5316=ORIENTED_EDGE('',*,*,#3955,.F.);
#5317=ORIENTED_EDGE('',*,*,#3940,.T.);
#5318=ORIENTED_EDGE('',*,*,#3952,.T.);
#5319=ORIENTED_EDGE('',*,*,#3947,.T.);
#5320=ORIENTED_EDGE('',*,*,#3944,.T.);
#5321=ORIENTED_EDGE('',*,*,#3958,.F.);
#5322=ORIENTED_EDGE('',*,*,#3959,.T.);
#5323=ORIENTED_EDGE('',*,*,#3960,.T.);
#5324=ORIENTED_EDGE('',*,*,#3959,.F.);
#5325=ORIENTED_EDGE('',*,*,#3958,.T.);
#5326=ORIENTED_EDGE('',*,*,#3957,.T.);
#5327=ORIENTED_EDGE('',*,*,#3960,.F.);
#5328=ORIENTED_EDGE('',*,*,#3953,.T.);
#5329=ORIENTED_EDGE('',*,*,#3961,.F.);
#5330=ORIENTED_EDGE('',*,*,#3962,.T.);
#5331=ORIENTED_EDGE('',*,*,#3963,.F.);
#5332=ORIENTED_EDGE('',*,*,#3962,.F.);
#5333=ORIENTED_EDGE('',*,*,#3964,.F.);
#5334=ORIENTED_EDGE('',*,*,#3965,.T.);
#5335=ORIENTED_EDGE('',*,*,#3966,.F.);
#5336=ORIENTED_EDGE('',*,*,#3967,.F.);
#5337=ORIENTED_EDGE('',*,*,#3968,.F.);
#5338=ORIENTED_EDGE('',*,*,#3969,.T.);
#5339=ORIENTED_EDGE('',*,*,#3970,.F.);
#5340=ORIENTED_EDGE('',*,*,#3965,.F.);
#5341=ORIENTED_EDGE('',*,*,#3971,.F.);
#5342=ORIENTED_EDGE('',*,*,#3972,.F.);
#5343=ORIENTED_EDGE('',*,*,#3973,.F.);
#5344=ORIENTED_EDGE('',*,*,#3969,.F.);
#5345=ORIENTED_EDGE('',*,*,#3974,.T.);
#5346=ORIENTED_EDGE('',*,*,#3966,.T.);
#5347=ORIENTED_EDGE('',*,*,#3970,.T.);
#5348=ORIENTED_EDGE('',*,*,#3973,.T.);
#5349=ORIENTED_EDGE('',*,*,#3975,.T.);
#5350=ORIENTED_EDGE('',*,*,#3967,.T.);
#5351=ORIENTED_EDGE('',*,*,#3975,.F.);
#5352=ORIENTED_EDGE('',*,*,#3972,.T.);
#5353=ORIENTED_EDGE('',*,*,#3976,.T.);
#5354=ORIENTED_EDGE('',*,*,#3977,.F.);
#5355=ORIENTED_EDGE('',*,*,#3978,.F.);
#5356=ORIENTED_EDGE('',*,*,#3979,.F.);
#5357=ORIENTED_EDGE('',*,*,#3980,.T.);
#5358=ORIENTED_EDGE('',*,*,#3980,.F.);
#5359=ORIENTED_EDGE('',*,*,#3981,.T.);
#5360=ORIENTED_EDGE('',*,*,#3982,.F.);
#5361=ORIENTED_EDGE('',*,*,#3983,.T.);
#5362=ORIENTED_EDGE('',*,*,#3961,.T.);
#5363=ORIENTED_EDGE('',*,*,#3979,.T.);
#5364=ORIENTED_EDGE('',*,*,#3984,.F.);
#5365=ORIENTED_EDGE('',*,*,#3985,.F.);
#5366=ORIENTED_EDGE('',*,*,#3981,.F.);
#5367=ORIENTED_EDGE('',*,*,#3977,.T.);
#5368=ORIENTED_EDGE('',*,*,#3983,.F.);
#5369=ORIENTED_EDGE('',*,*,#3986,.F.);
#5370=ORIENTED_EDGE('',*,*,#3987,.F.);
#5371=ORIENTED_EDGE('',*,*,#3987,.T.);
#5372=ORIENTED_EDGE('',*,*,#3988,.F.);
#5373=ORIENTED_EDGE('',*,*,#3984,.T.);
#5374=ORIENTED_EDGE('',*,*,#3978,.T.);
#5375=ORIENTED_EDGE('',*,*,#3963,.T.);
#5376=ORIENTED_EDGE('',*,*,#3974,.F.);
#5377=ORIENTED_EDGE('',*,*,#3989,.T.);
#5378=ORIENTED_EDGE('',*,*,#3990,.T.);
#5379=ORIENTED_EDGE('',*,*,#3989,.F.);
#5380=ORIENTED_EDGE('',*,*,#3985,.T.);
#5381=ORIENTED_EDGE('',*,*,#3988,.T.);
#5382=ORIENTED_EDGE('',*,*,#3986,.T.);
#5383=ORIENTED_EDGE('',*,*,#3982,.T.);
#5384=ORIENTED_EDGE('',*,*,#3990,.F.);
#5385=ORIENTED_EDGE('',*,*,#3964,.T.);
#5386=ORIENTED_EDGE('',*,*,#3976,.F.);
#5387=ORIENTED_EDGE('',*,*,#3971,.T.);
#5388=ORIENTED_EDGE('',*,*,#3968,.T.);
#5389=ORIENTED_EDGE('',*,*,#3991,.F.);
#5390=ORIENTED_EDGE('',*,*,#3992,.T.);
#5391=ORIENTED_EDGE('',*,*,#3993,.T.);
#5392=ORIENTED_EDGE('',*,*,#3992,.F.);
#5393=ORIENTED_EDGE('',*,*,#3993,.F.);
#5394=ORIENTED_EDGE('',*,*,#3994,.F.);
#5395=ORIENTED_EDGE('',*,*,#3995,.T.);
#5396=ORIENTED_EDGE('',*,*,#3996,.T.);
#5397=ORIENTED_EDGE('',*,*,#3995,.F.);
#5398=ORIENTED_EDGE('',*,*,#3994,.T.);
#5399=ORIENTED_EDGE('',*,*,#3996,.F.);
#5400=ORIENTED_EDGE('',*,*,#3991,.T.);
#5401=ORIENTED_EDGE('',*,*,#3997,.F.);
#5402=ORIENTED_EDGE('',*,*,#3998,.T.);
#5403=ORIENTED_EDGE('',*,*,#3999,.T.);
#5404=ORIENTED_EDGE('',*,*,#3998,.F.);
#5405=ORIENTED_EDGE('',*,*,#4000,.F.);
#5406=ORIENTED_EDGE('',*,*,#4001,.T.);
#5407=ORIENTED_EDGE('',*,*,#4002,.T.);
#5408=ORIENTED_EDGE('',*,*,#4001,.F.);
#5409=ORIENTED_EDGE('',*,*,#4000,.T.);
#5410=ORIENTED_EDGE('',*,*,#3997,.T.);
#5411=ORIENTED_EDGE('',*,*,#4002,.F.);
#5412=ORIENTED_EDGE('',*,*,#3999,.F.);
#5413=ORIENTED_EDGE('',*,*,#4003,.F.);
#5414=ORIENTED_EDGE('',*,*,#4004,.T.);
#5415=ORIENTED_EDGE('',*,*,#4005,.T.);
#5416=ORIENTED_EDGE('',*,*,#4004,.F.);
#5417=ORIENTED_EDGE('',*,*,#4006,.F.);
#5418=ORIENTED_EDGE('',*,*,#4007,.T.);
#5419=ORIENTED_EDGE('',*,*,#4008,.T.);
#5420=ORIENTED_EDGE('',*,*,#4007,.F.);
#5421=ORIENTED_EDGE('',*,*,#4006,.T.);
#5422=ORIENTED_EDGE('',*,*,#4003,.T.);
#5423=ORIENTED_EDGE('',*,*,#4008,.F.);
#5424=ORIENTED_EDGE('',*,*,#4005,.F.);
#5425=ORIENTED_EDGE('',*,*,#4009,.F.);
#5426=ORIENTED_EDGE('',*,*,#4010,.F.);
#5427=ORIENTED_EDGE('',*,*,#4011,.F.);
#5428=ORIENTED_EDGE('',*,*,#4012,.F.);
#5429=ORIENTED_EDGE('',*,*,#4013,.F.);
#5430=ORIENTED_EDGE('',*,*,#4014,.F.);
#5431=ORIENTED_EDGE('',*,*,#4015,.F.);
#5432=ORIENTED_EDGE('',*,*,#4016,.F.);
#5433=ORIENTED_EDGE('',*,*,#4013,.T.);
#5434=ORIENTED_EDGE('',*,*,#4017,.T.);
#5435=ORIENTED_EDGE('',*,*,#4018,.T.);
#5436=ORIENTED_EDGE('',*,*,#4019,.T.);
#5437=ORIENTED_EDGE('',*,*,#4012,.T.);
#5438=ORIENTED_EDGE('',*,*,#4020,.F.);
#5439=ORIENTED_EDGE('',*,*,#4021,.T.);
#5440=ORIENTED_EDGE('',*,*,#4017,.F.);
#5441=ORIENTED_EDGE('',*,*,#4011,.T.);
#5442=ORIENTED_EDGE('',*,*,#4022,.T.);
#5443=ORIENTED_EDGE('',*,*,#4023,.T.);
#5444=ORIENTED_EDGE('',*,*,#4020,.T.);
#5445=ORIENTED_EDGE('',*,*,#4010,.T.);
#5446=ORIENTED_EDGE('',*,*,#4024,.F.);
#5447=ORIENTED_EDGE('',*,*,#4025,.T.);
#5448=ORIENTED_EDGE('',*,*,#4022,.F.);
#5449=ORIENTED_EDGE('',*,*,#4018,.F.);
#5450=ORIENTED_EDGE('',*,*,#4021,.F.);
#5451=ORIENTED_EDGE('',*,*,#4023,.F.);
#5452=ORIENTED_EDGE('',*,*,#4025,.F.);
#5453=ORIENTED_EDGE('',*,*,#4026,.F.);
#5454=ORIENTED_EDGE('',*,*,#4027,.F.);
#5455=ORIENTED_EDGE('',*,*,#4028,.F.);
#5456=ORIENTED_EDGE('',*,*,#4029,.F.);
#5457=ORIENTED_EDGE('',*,*,#4009,.T.);
#5458=ORIENTED_EDGE('',*,*,#4030,.T.);
#5459=ORIENTED_EDGE('',*,*,#4026,.T.);
#5460=ORIENTED_EDGE('',*,*,#4024,.T.);
#5461=ORIENTED_EDGE('',*,*,#4016,.T.);
#5462=ORIENTED_EDGE('',*,*,#4031,.F.);
#5463=ORIENTED_EDGE('',*,*,#4027,.T.);
#5464=ORIENTED_EDGE('',*,*,#4030,.F.);
#5465=ORIENTED_EDGE('',*,*,#4015,.T.);
#5466=ORIENTED_EDGE('',*,*,#4032,.T.);
#5467=ORIENTED_EDGE('',*,*,#4028,.T.);
#5468=ORIENTED_EDGE('',*,*,#4031,.T.);
#5469=ORIENTED_EDGE('',*,*,#4014,.T.);
#5470=ORIENTED_EDGE('',*,*,#4019,.F.);
#5471=ORIENTED_EDGE('',*,*,#4029,.T.);
#5472=ORIENTED_EDGE('',*,*,#4032,.F.);
#5473=ORIENTED_EDGE('',*,*,#4033,.F.);
#5474=ORIENTED_EDGE('',*,*,#4034,.F.);
#5475=ORIENTED_EDGE('',*,*,#4035,.T.);
#5476=ORIENTED_EDGE('',*,*,#4033,.T.);
#5477=ORIENTED_EDGE('',*,*,#4035,.F.);
#5478=ORIENTED_EDGE('',*,*,#4036,.F.);
#5479=ORIENTED_EDGE('',*,*,#4037,.T.);
#5480=ORIENTED_EDGE('',*,*,#4034,.T.);
#5481=ORIENTED_EDGE('',*,*,#4037,.F.);
#5482=ORIENTED_EDGE('',*,*,#4038,.F.);
#5483=ORIENTED_EDGE('',*,*,#4039,.T.);
#5484=ORIENTED_EDGE('',*,*,#4036,.T.);
#5485=ORIENTED_EDGE('',*,*,#4039,.F.);
#5486=ORIENTED_EDGE('',*,*,#4038,.T.);
#5487=ORIENTED_EDGE('',*,*,#4040,.F.);
#5488=ORIENTED_EDGE('',*,*,#4041,.F.);
#5489=ORIENTED_EDGE('',*,*,#4042,.T.);
#5490=ORIENTED_EDGE('',*,*,#4040,.T.);
#5491=ORIENTED_EDGE('',*,*,#4042,.F.);
#5492=ORIENTED_EDGE('',*,*,#4043,.F.);
#5493=ORIENTED_EDGE('',*,*,#4044,.T.);
#5494=ORIENTED_EDGE('',*,*,#4041,.T.);
#5495=ORIENTED_EDGE('',*,*,#4044,.F.);
#5496=ORIENTED_EDGE('',*,*,#4045,.F.);
#5497=ORIENTED_EDGE('',*,*,#4046,.T.);
#5498=ORIENTED_EDGE('',*,*,#4043,.T.);
#5499=ORIENTED_EDGE('',*,*,#4046,.F.);
#5500=ORIENTED_EDGE('',*,*,#4045,.T.);
#5501=ORIENTED_EDGE('',*,*,#4047,.T.);
#5502=ORIENTED_EDGE('',*,*,#4048,.T.);
#5503=ORIENTED_EDGE('',*,*,#4049,.T.);
#5504=ORIENTED_EDGE('',*,*,#4050,.F.);
#5505=ORIENTED_EDGE('',*,*,#4051,.T.);
#5506=ORIENTED_EDGE('',*,*,#4052,.T.);
#5507=ORIENTED_EDGE('',*,*,#4053,.T.);
#5508=ORIENTED_EDGE('',*,*,#4048,.F.);
#5509=ORIENTED_EDGE('',*,*,#4054,.T.);
#5510=ORIENTED_EDGE('',*,*,#4055,.T.);
#5511=ORIENTED_EDGE('',*,*,#4056,.T.);
#5512=ORIENTED_EDGE('',*,*,#4052,.F.);
#5513=ORIENTED_EDGE('',*,*,#4057,.T.);
#5514=ORIENTED_EDGE('',*,*,#4058,.T.);
#5515=ORIENTED_EDGE('',*,*,#4059,.T.);
#5516=ORIENTED_EDGE('',*,*,#4055,.F.);
#5517=ORIENTED_EDGE('',*,*,#4060,.T.);
#5518=ORIENTED_EDGE('',*,*,#4061,.T.);
#5519=ORIENTED_EDGE('',*,*,#4062,.T.);
#5520=ORIENTED_EDGE('',*,*,#4058,.F.);
#5521=ORIENTED_EDGE('',*,*,#4063,.T.);
#5522=ORIENTED_EDGE('',*,*,#4050,.T.);
#5523=ORIENTED_EDGE('',*,*,#4064,.T.);
#5524=ORIENTED_EDGE('',*,*,#4061,.F.);
#5525=ORIENTED_EDGE('',*,*,#4063,.F.);
#5526=ORIENTED_EDGE('',*,*,#4060,.F.);
#5527=ORIENTED_EDGE('',*,*,#4057,.F.);
#5528=ORIENTED_EDGE('',*,*,#4054,.F.);
#5529=ORIENTED_EDGE('',*,*,#4051,.F.);
#5530=ORIENTED_EDGE('',*,*,#4047,.F.);
#5531=ORIENTED_EDGE('',*,*,#4064,.F.);
#5532=ORIENTED_EDGE('',*,*,#4049,.F.);
#5533=ORIENTED_EDGE('',*,*,#4053,.F.);
#5534=ORIENTED_EDGE('',*,*,#4056,.F.);
#5535=ORIENTED_EDGE('',*,*,#4059,.F.);
#5536=ORIENTED_EDGE('',*,*,#4062,.F.);
#5537=ORIENTED_EDGE('',*,*,#4065,.F.);
#5538=ORIENTED_EDGE('',*,*,#4066,.T.);
#5539=ORIENTED_EDGE('',*,*,#4067,.F.);
#5540=ORIENTED_EDGE('',*,*,#4066,.F.);
#5541=ORIENTED_EDGE('',*,*,#4068,.T.);
#5542=ORIENTED_EDGE('',*,*,#4069,.T.);
#5543=ORIENTED_EDGE('',*,*,#4070,.F.);
#5544=ORIENTED_EDGE('',*,*,#4071,.F.);
#5545=ORIENTED_EDGE('',*,*,#4072,.T.);
#5546=ORIENTED_EDGE('',*,*,#4071,.T.);
#5547=ORIENTED_EDGE('',*,*,#4073,.F.);
#5548=ORIENTED_EDGE('',*,*,#4074,.F.);
#5549=ORIENTED_EDGE('',*,*,#4075,.T.);
#5550=ORIENTED_EDGE('',*,*,#4074,.T.);
#5551=ORIENTED_EDGE('',*,*,#4076,.F.);
#5552=ORIENTED_EDGE('',*,*,#4077,.F.);
#5553=ORIENTED_EDGE('',*,*,#4078,.T.);
#5554=ORIENTED_EDGE('',*,*,#4077,.T.);
#5555=ORIENTED_EDGE('',*,*,#4079,.F.);
#5556=ORIENTED_EDGE('',*,*,#4069,.F.);
#5557=ORIENTED_EDGE('',*,*,#4079,.T.);
#5558=ORIENTED_EDGE('',*,*,#4076,.T.);
#5559=ORIENTED_EDGE('',*,*,#4073,.T.);
#5560=ORIENTED_EDGE('',*,*,#4070,.T.);
#5561=ORIENTED_EDGE('',*,*,#4067,.T.);
#5562=ORIENTED_EDGE('',*,*,#4078,.F.);
#5563=ORIENTED_EDGE('',*,*,#4068,.F.);
#5564=ORIENTED_EDGE('',*,*,#4072,.F.);
#5565=ORIENTED_EDGE('',*,*,#4075,.F.);
#5566=ORIENTED_EDGE('',*,*,#4065,.T.);
#5567=ORIENTED_EDGE('',*,*,#4080,.F.);
#5568=ORIENTED_EDGE('',*,*,#4081,.T.);
#5569=ORIENTED_EDGE('',*,*,#4082,.F.);
#5570=ORIENTED_EDGE('',*,*,#4083,.T.);
#5571=ORIENTED_EDGE('',*,*,#4080,.T.);
#5572=ORIENTED_EDGE('',*,*,#4083,.F.);
#5573=ORIENTED_EDGE('',*,*,#4082,.T.);
#5574=ORIENTED_EDGE('',*,*,#4084,.F.);
#5575=ORIENTED_EDGE('',*,*,#4085,.T.);
#5576=ORIENTED_EDGE('',*,*,#4086,.T.);
#5577=ORIENTED_EDGE('',*,*,#4085,.F.);
#5578=ORIENTED_EDGE('',*,*,#4086,.F.);
#5579=ORIENTED_EDGE('',*,*,#4081,.F.);
#5580=ORIENTED_EDGE('',*,*,#4087,.T.);
#5581=ORIENTED_EDGE('',*,*,#4088,.T.);
#5582=ORIENTED_EDGE('',*,*,#4087,.F.);
#5583=ORIENTED_EDGE('',*,*,#4088,.F.);
#5584=ORIENTED_EDGE('',*,*,#4084,.T.);
#5585=ORIENTED_EDGE('',*,*,#4089,.F.);
#5586=ORIENTED_EDGE('',*,*,#4090,.T.);
#5587=ORIENTED_EDGE('',*,*,#4091,.T.);
#5588=ORIENTED_EDGE('',*,*,#4090,.F.);
#5589=ORIENTED_EDGE('',*,*,#4092,.F.);
#5590=ORIENTED_EDGE('',*,*,#4093,.T.);
#5591=ORIENTED_EDGE('',*,*,#4094,.T.);
#5592=ORIENTED_EDGE('',*,*,#4093,.F.);
#5593=ORIENTED_EDGE('',*,*,#4092,.T.);
#5594=ORIENTED_EDGE('',*,*,#4089,.T.);
#5595=ORIENTED_EDGE('',*,*,#4094,.F.);
#5596=ORIENTED_EDGE('',*,*,#4091,.F.);
#5597=PLANE('',#6625);
#5598=PLANE('',#6626);
#5599=PLANE('',#6627);
#5600=PLANE('',#6628);
#5601=PLANE('',#6629);
#5602=PLANE('',#6648);
#5603=PLANE('',#6649);
#5604=PLANE('',#6650);
#5605=PLANE('',#6651);
#5606=PLANE('',#6652);
#5607=PLANE('',#6653);
#5608=PLANE('',#6655);
#5609=PLANE('',#6656);
#5610=PLANE('',#6657);
#5611=PLANE('',#6658);
#5612=PLANE('',#6659);
#5613=PLANE('',#6660);
#5614=PLANE('',#6662);
#5615=PLANE('',#6663);
#5616=PLANE('',#6664);
#5617=PLANE('',#6665);
#5618=PLANE('',#6666);
#5619=PLANE('',#6667);
#5620=PLANE('',#6690);
#5621=PLANE('',#6691);
#5622=PLANE('',#6692);
#5623=PLANE('',#6693);
#5624=PLANE('',#6694);
#5625=PLANE('',#6695);
#5626=PLANE('',#6696);
#5627=PLANE('',#6697);
#5628=PLANE('',#6698);
#5629=PLANE('',#6699);
#5630=PLANE('',#6716);
#5631=PLANE('',#6723);
#5632=PLANE('',#6724);
#5633=PLANE('',#6741);
#5634=PLANE('',#6748);
#5635=PLANE('',#6749);
#5636=PLANE('',#6772);
#5637=PLANE('',#6773);
#5638=PLANE('',#6774);
#5639=PLANE('',#6775);
#5640=PLANE('',#6776);
#5641=PLANE('',#6777);
#5642=PLANE('',#6778);
#5643=PLANE('',#6779);
#5644=PLANE('',#6780);
#5645=PLANE('',#6781);
#5646=PLANE('',#6798);
#5647=PLANE('',#6805);
#5648=PLANE('',#6806);
#5649=PLANE('',#6823);
#5650=PLANE('',#6830);
#5651=PLANE('',#6831);
#5652=PLANE('',#6836);
#5653=PLANE('',#6840);
#5654=PLANE('',#6844);
#5655=PLANE('',#6848);
#5656=PLANE('',#6852);
#5657=PLANE('',#6859);
#5658=PLANE('',#6866);
#5659=PLANE('',#6870);
#5660=PLANE('',#6871);
#5661=PLANE('',#6872);
#5662=PLANE('',#6873);
#5663=PLANE('',#6874);
#5664=PLANE('',#6875);
#5665=PLANE('',#6876);
#5666=PLANE('',#6877);
#5667=PLANE('',#6878);
#5668=PLANE('',#6879);
#5669=PLANE('',#6880);
#5670=PLANE('',#6881);
#5671=PLANE('',#6882);
#5672=PLANE('',#6883);
#5673=PLANE('',#6900);
#5674=PLANE('',#6907);
#5675=PLANE('',#6908);
#5676=PLANE('',#6912);
#5677=PLANE('',#6913);
#5678=PLANE('',#6929);
#5679=PLANE('',#6932);
#5680=PLANE('',#6944);
#5681=PLANE('',#6953);
#5682=PLANE('',#6984);
#5683=PLANE('',#6989);
#5684=PLANE('',#6994);
#5685=PLANE('',#7000);
#5686=PLANE('',#7005);
#5687=PLANE('',#7014);
#5688=PLANE('',#7018);
#5689=PLANE('',#7019);
#5690=PLANE('',#7021);
#5691=PLANE('',#7026);
#5692=PLANE('',#7029);
#5693=PLANE('',#7034);
#5694=PLANE('',#7043);
#5695=PLANE('',#7051);
#5696=PLANE('',#7059);
#5697=PLANE('',#7060);
#5698=PLANE('',#7061);
#5699=PLANE('',#7062);
#5700=PLANE('',#7063);
#5701=PLANE('',#7064);
#5702=PLANE('',#7065);
#5703=PLANE('',#7066);
#5704=PLANE('',#7067);
#5705=PLANE('',#7070);
#5706=PLANE('',#7072);
#5707=PLANE('',#7073);
#5708=PLANE('',#7075);
#5709=PLANE('',#7076);
#5710=PLANE('',#7077);
#5711=PLANE('',#7082);
#5712=PLANE('',#7086);
#5713=PLANE('',#7090);
#5714=PLANE('',#7094);
#5715=PLANE('',#7098);
#5716=PLANE('',#7102);
#5717=PLANE('',#7105);
#5718=PLANE('',#7106);
#5719=PLANE('',#7109);
#5720=PLANE('',#7110);
#5721=PLANE('',#7115);
#5722=PLANE('',#7121);
#5723=PLANE('',#7122);
#5724=PLANE('',#7123);
#5725=PLANE('',#7124);
#5726=PLANE('',#7125);
#5727=PLANE('',#7126);
#5728=PLANE('',#7127);
#5729=PLANE('',#7128);
#5730=PLANE('',#7129);
#5731=PLANE('',#7131);
#5732=PLANE('',#7139);
#5733=PLANE('',#7149);
#5734=PLANE('',#7153);
#5735=PLANE('',#7154);
#5736=PLANE('',#7155);
#5737=PLANE('',#7157);
#5738=PLANE('',#7158);
#5739=PLANE('',#7159);
#5740=PLANE('',#7161);
#5741=PLANE('',#7162);
#5742=PLANE('',#7164);
#5743=PLANE('',#7165);
#5744=PLANE('',#7166);
#5745=PLANE('',#7171);
#5746=PLANE('',#7172);
#5747=PLANE('',#7180);
#5748=PLANE('',#7181);
#5749=PLANE('',#7189);
#5750=PLANE('',#7190);
#5751=PLANE('',#7198);
#5752=PLANE('',#7199);
#5753=PLANE('',#7207);
#5754=PLANE('',#7208);
#5755=PLANE('',#7210);
#5756=PLANE('',#7211);
#5757=PLANE('',#7212);
#5758=PLANE('',#7213);
#5759=PLANE('',#7223);
#5760=PLANE('',#7227);
#5761=PLANE('',#7228);
#5762=PLANE('',#7233);
#5763=PLANE('',#7234);
#5764=PLANE('',#7235);
#5765=PLANE('',#7236);
#5766=PLANE('',#7244);
#5767=PLANE('',#7246);
#5768=PLANE('',#7247);
#5769=PLANE('',#7248);
#5770=PLANE('',#7252);
#5771=PLANE('',#7257);
#5772=PLANE('',#7261);
#5773=PLANE('',#7262);
#5774=PLANE('',#7270);
#5775=PLANE('',#7271);
#5776=PLANE('',#7279);
#5777=PLANE('',#7280);
#5778=PLANE('',#7282);
#5779=PLANE('',#7283);
#5780=PLANE('',#7284);
#5781=PLANE('',#7285);
#5782=PLANE('',#7286);
#5783=PLANE('',#7287);
#5784=PLANE('',#7288);
#5785=PLANE('',#7289);
#5786=PLANE('',#7290);
#5787=PLANE('',#7291);
#5788=PLANE('',#7293);
#5789=PLANE('',#7301);
#5790=PLANE('',#7309);
#5791=PLANE('',#7310);
#5792=PLANE('',#7311);
#5793=PLANE('',#7312);
#5794=PLANE('',#7313);
#5795=PLANE('',#7314);
#5796=PLANE('',#7315);
#5797=PLANE('',#7316);
#5798=PLANE('',#7317);
#5799=PLANE('',#7379);
#5800=PLANE('',#7380);
#5801=PLANE('',#7381);
#5802=PLANE('',#7382);
#5803=PLANE('',#7383);
#5804=PLANE('',#7384);
#5805=PLANE('',#7386);
#5806=PLANE('',#7391);
#5807=PLANE('',#7395);
#5808=PLANE('',#7398);
#5809=PLANE('',#7406);
#5810=PLANE('',#7407);
#5811=ADVANCED_FACE('',(#1095),#5597,.F.);
#5812=ADVANCED_FACE('',(#1096),#5598,.F.);
#5813=ADVANCED_FACE('',(#1097),#5599,.F.);
#5814=ADVANCED_FACE('',(#1098),#5600,.F.);
#5815=ADVANCED_FACE('',(#1099),#5601,.T.);
#5816=ADVANCED_FACE('',(#1100),#973,.F.);
#5817=ADVANCED_FACE('',(#1101),#974,.F.);
#5818=ADVANCED_FACE('',(#1102),#975,.F.);
#5819=ADVANCED_FACE('',(#1103),#976,.F.);
#5820=ADVANCED_FACE('',(#1104),#977,.F.);
#5821=ADVANCED_FACE('',(#1105),#978,.F.);
#5822=ADVANCED_FACE('',(#1106),#5602,.T.);
#5823=ADVANCED_FACE('',(#1107),#5603,.T.);
#5824=ADVANCED_FACE('',(#1108),#5604,.T.);
#5825=ADVANCED_FACE('',(#1109),#5605,.T.);
#5826=ADVANCED_FACE('',(#1110,#495,#496,#497,#498,#499,#500,#501),#5606,
 .T.);
#5827=ADVANCED_FACE('',(#1111,#502,#503,#504,#505,#506,#507),#5607,.F.);
#5828=ADVANCED_FACE('',(#1112),#5608,.T.);
#5829=ADVANCED_FACE('',(#1113),#5609,.T.);
#5830=ADVANCED_FACE('',(#1114),#5610,.T.);
#5831=ADVANCED_FACE('',(#1115),#5611,.T.);
#5832=ADVANCED_FACE('',(#1116),#5612,.T.);
#5833=ADVANCED_FACE('',(#1117),#5613,.F.);
#5834=ADVANCED_FACE('',(#1118),#5614,.T.);
#5835=ADVANCED_FACE('',(#1119),#5615,.T.);
#5836=ADVANCED_FACE('',(#1120),#5616,.T.);
#5837=ADVANCED_FACE('',(#1121),#5617,.T.);
#5838=ADVANCED_FACE('',(#1122),#5618,.T.);
#5839=ADVANCED_FACE('',(#1123),#5619,.F.);
#5840=ADVANCED_FACE('',(#1124),#979,.F.);
#5841=ADVANCED_FACE('',(#1125),#980,.F.);
#5842=ADVANCED_FACE('',(#1126),#981,.F.);
#5843=ADVANCED_FACE('',(#1127),#982,.F.);
#5844=ADVANCED_FACE('',(#1128),#983,.F.);
#5845=ADVANCED_FACE('',(#1129),#984,.F.);
#5846=ADVANCED_FACE('',(#1130),#985,.F.);
#5847=ADVANCED_FACE('',(#1131,#508),#5620,.T.);
#5848=ADVANCED_FACE('',(#1132,#509),#5621,.T.);
#5849=ADVANCED_FACE('',(#1133),#5622,.T.);
#5850=ADVANCED_FACE('',(#1134),#5623,.T.);
#5851=ADVANCED_FACE('',(#1135,#510,#511,#512,#513,#514),#5624,.T.);
#5852=ADVANCED_FACE('',(#1136),#5625,.T.);
#5853=ADVANCED_FACE('',(#1137,#515,#516,#517,#518,#519),#5626,.T.);
#5854=ADVANCED_FACE('',(#1138),#5627,.T.);
#5855=ADVANCED_FACE('',(#1139),#5628,.T.);
#5856=ADVANCED_FACE('',(#1140,#520,#521),#5629,.F.);
#5857=ADVANCED_FACE('',(#1141),#986,.F.);
#5858=ADVANCED_FACE('',(#1142),#987,.F.);
#5859=ADVANCED_FACE('',(#1143),#988,.F.);
#5860=ADVANCED_FACE('',(#1144),#989,.F.);
#5861=ADVANCED_FACE('',(#1145),#990,.T.);
#5862=ADVANCED_FACE('',(#1146,#522),#5630,.T.);
#5863=ADVANCED_FACE('',(#1147),#991,.F.);
#5864=ADVANCED_FACE('',(#1148),#992,.T.);
#5865=ADVANCED_FACE('',(#1149,#523,#524,#525,#526,#527),#5631,.T.);
#5866=ADVANCED_FACE('',(#1150,#528,#529,#530,#531,#532),#5632,.F.);
#5867=ADVANCED_FACE('',(#1151),#993,.F.);
#5868=ADVANCED_FACE('',(#1152),#994,.F.);
#5869=ADVANCED_FACE('',(#1153),#995,.F.);
#5870=ADVANCED_FACE('',(#1154),#996,.F.);
#5871=ADVANCED_FACE('',(#1155),#997,.T.);
#5872=ADVANCED_FACE('',(#1156,#533),#5633,.F.);
#5873=ADVANCED_FACE('',(#1157),#998,.F.);
#5874=ADVANCED_FACE('',(#1158),#999,.T.);
#5875=ADVANCED_FACE('',(#1159,#534,#535,#536,#537,#538),#5634,.T.);
#5876=ADVANCED_FACE('',(#1160,#539,#540,#541,#542,#543),#5635,.F.);
#5877=ADVANCED_FACE('',(#1161),#1000,.F.);
#5878=ADVANCED_FACE('',(#1162),#1001,.F.);
#5879=ADVANCED_FACE('',(#1163),#1002,.F.);
#5880=ADVANCED_FACE('',(#1164),#1003,.F.);
#5881=ADVANCED_FACE('',(#1165),#1004,.F.);
#5882=ADVANCED_FACE('',(#1166),#1005,.F.);
#5883=ADVANCED_FACE('',(#1167),#1006,.F.);
#5884=ADVANCED_FACE('',(#1168,#544),#5636,.T.);
#5885=ADVANCED_FACE('',(#1169,#545),#5637,.T.);
#5886=ADVANCED_FACE('',(#1170),#5638,.T.);
#5887=ADVANCED_FACE('',(#1171),#5639,.T.);
#5888=ADVANCED_FACE('',(#1172,#546,#547,#548,#549,#550),#5640,.T.);
#5889=ADVANCED_FACE('',(#1173),#5641,.T.);
#5890=ADVANCED_FACE('',(#1174,#551,#552,#553,#554,#555),#5642,.T.);
#5891=ADVANCED_FACE('',(#1175),#5643,.T.);
#5892=ADVANCED_FACE('',(#1176),#5644,.T.);
#5893=ADVANCED_FACE('',(#1177,#556,#557),#5645,.F.);
#5894=ADVANCED_FACE('',(#1178),#1007,.F.);
#5895=ADVANCED_FACE('',(#1179),#1008,.F.);
#5896=ADVANCED_FACE('',(#1180),#1009,.F.);
#5897=ADVANCED_FACE('',(#1181),#1010,.F.);
#5898=ADVANCED_FACE('',(#1182),#1011,.T.);
#5899=ADVANCED_FACE('',(#1183,#558),#5646,.T.);
#5900=ADVANCED_FACE('',(#1184),#1012,.F.);
#5901=ADVANCED_FACE('',(#1185),#1013,.T.);
#5902=ADVANCED_FACE('',(#1186,#559,#560,#561,#562,#563),#5647,.T.);
#5903=ADVANCED_FACE('',(#1187,#564,#565,#566,#567,#568),#5648,.F.);
#5904=ADVANCED_FACE('',(#1188),#1014,.F.);
#5905=ADVANCED_FACE('',(#1189),#1015,.F.);
#5906=ADVANCED_FACE('',(#1190),#1016,.F.);
#5907=ADVANCED_FACE('',(#1191),#1017,.F.);
#5908=ADVANCED_FACE('',(#1192),#1018,.T.);
#5909=ADVANCED_FACE('',(#1193,#569),#5649,.F.);
#5910=ADVANCED_FACE('',(#1194),#1019,.F.);
#5911=ADVANCED_FACE('',(#1195),#1020,.T.);
#5912=ADVANCED_FACE('',(#1196,#570,#571,#572,#573,#574),#5650,.T.);
#5913=ADVANCED_FACE('',(#1197,#575,#576,#577,#578,#579),#5651,.F.);
#5914=ADVANCED_FACE('',(#1198),#1021,.F.);
#5915=ADVANCED_FACE('',(#1199),#5652,.T.);
#5916=ADVANCED_FACE('',(#1200),#1022,.F.);
#5917=ADVANCED_FACE('',(#1201),#5653,.T.);
#5918=ADVANCED_FACE('',(#1202),#1023,.F.);
#5919=ADVANCED_FACE('',(#1203),#5654,.T.);
#5920=ADVANCED_FACE('',(#1204),#1024,.F.);
#5921=ADVANCED_FACE('',(#1205),#5655,.T.);
#5922=ADVANCED_FACE('',(#1206),#1025,.F.);
#5923=ADVANCED_FACE('',(#1207,#580),#5656,.T.);
#5924=ADVANCED_FACE('',(#1208),#1026,.F.);
#5925=ADVANCED_FACE('',(#1209),#1027,.F.);
#5926=ADVANCED_FACE('',(#1210,#581),#5657,.T.);
#5927=ADVANCED_FACE('',(#1211),#1028,.F.);
#5928=ADVANCED_FACE('',(#1212),#1029,.F.);
#5929=ADVANCED_FACE('',(#1213,#582),#5658,.T.);
#5930=ADVANCED_FACE('',(#1214),#1030,.F.);
#5931=ADVANCED_FACE('',(#1215,#583),#5659,.T.);
#5932=ADVANCED_FACE('',(#1216),#5660,.T.);
#5933=ADVANCED_FACE('',(#1217),#5661,.F.);
#5934=ADVANCED_FACE('',(#1218),#5662,.T.);
#5935=ADVANCED_FACE('',(#1219),#5663,.T.);
#5936=ADVANCED_FACE('',(#1220,#584),#5664,.T.);
#5937=ADVANCED_FACE('',(#1221),#5665,.T.);
#5938=ADVANCED_FACE('',(#1222),#5666,.F.);
#5939=ADVANCED_FACE('',(#1223),#5667,.T.);
#5940=ADVANCED_FACE('',(#1224),#5668,.T.);
#5941=ADVANCED_FACE('',(#1225),#5669,.T.);
#5942=ADVANCED_FACE('',(#1226),#5670,.T.);
#5943=ADVANCED_FACE('',(#1227,#585,#586,#587,#588,#589,#590,#591),#5671,
 .T.);
#5944=ADVANCED_FACE('',(#1228,#592),#5672,.F.);
#5945=ADVANCED_FACE('',(#1229),#1031,.F.);
#5946=ADVANCED_FACE('',(#1230),#1032,.F.);
#5947=ADVANCED_FACE('',(#1231),#1033,.F.);
#5948=ADVANCED_FACE('',(#1232),#1034,.F.);
#5949=ADVANCED_FACE('',(#1233),#1035,.T.);
#5950=ADVANCED_FACE('',(#1234,#593),#5673,.F.);
#5951=ADVANCED_FACE('',(#1235),#1036,.F.);
#5952=ADVANCED_FACE('',(#1236),#1037,.T.);
#5953=ADVANCED_FACE('',(#1237,#594,#595,#596,#597,#598),#5674,.T.);
#5954=ADVANCED_FACE('',(#1238,#599,#600,#601,#602,#603),#5675,.F.);
#5955=ADVANCED_FACE('',(#1239),#339,.T.);
#5956=ADVANCED_FACE('',(#1240),#5676,.T.);
#5957=ADVANCED_FACE('',(#1241),#5677,.F.);
#5958=ADVANCED_FACE('',(#1242),#322,.F.);
#5959=ADVANCED_FACE('',(#1243),#1038,.T.);
#5960=ADVANCED_FACE('',(#1244),#1039,.F.);
#5961=ADVANCED_FACE('',(#1245),#307,.F.);
#5962=ADVANCED_FACE('',(#1246,#604),#5678,.T.);
#5963=ADVANCED_FACE('',(#1247),#1040,.T.);
#5964=ADVANCED_FACE('',(#1248,#605),#5679,.T.);
#5965=ADVANCED_FACE('',(#1249),#308,.F.);
#5966=ADVANCED_FACE('',(#1250),#323,.F.);
#5967=ADVANCED_FACE('',(#1251),#1041,.F.);
#5968=ADVANCED_FACE('',(#1252,#606),#5680,.T.);
#5969=ADVANCED_FACE('',(#1253),#309,.T.);
#5970=ADVANCED_FACE('',(#1254),#1042,.T.);
#5971=ADVANCED_FACE('',(#1255),#310,.T.);
#5972=ADVANCED_FACE('',(#1256,#607),#5681,.T.);
#5973=ADVANCED_FACE('',(#1257),#1043,.F.);
#5974=ADVANCED_FACE('',(#1258),#293,.T.);
#5975=ADVANCED_FACE('',(#1259),#294,.T.);
#5976=ADVANCED_FACE('',(#1260),#295,.T.);
#5977=ADVANCED_FACE('',(#1261),#296,.T.);
#5978=ADVANCED_FACE('',(#1262),#297,.T.);
#5979=ADVANCED_FACE('',(#1263),#298,.T.);
#5980=ADVANCED_FACE('',(#1264),#299,.T.);
#5981=ADVANCED_FACE('',(#1265),#300,.F.);
#5982=ADVANCED_FACE('',(#1266),#1044,.T.);
#5983=ADVANCED_FACE('',(#1267),#5682,.T.);
#5984=ADVANCED_FACE('',(#1268),#301,.F.);
#5985=ADVANCED_FACE('',(#1269),#5683,.T.);
#5986=ADVANCED_FACE('',(#1270),#302,.F.);
#5987=ADVANCED_FACE('',(#1271),#5684,.T.);
#5988=ADVANCED_FACE('',(#1272),#303,.F.);
#5989=ADVANCED_FACE('',(#1273),#5685,.T.);
#5990=ADVANCED_FACE('',(#1274),#304,.F.);
#5991=ADVANCED_FACE('',(#1275),#5686,.T.);
#5992=ADVANCED_FACE('',(#1276),#305,.F.);
#5993=ADVANCED_FACE('',(#1277),#1045,.F.);
#5994=ADVANCED_FACE('',(#1278),#5687,.T.);
#5995=ADVANCED_FACE('',(#1279),#306,.F.);
#5996=ADVANCED_FACE('',(#1280,#608),#5688,.T.);
#5997=ADVANCED_FACE('',(#1281),#5689,.T.);
#5998=ADVANCED_FACE('',(#1282,#609),#5690,.T.);
#5999=ADVANCED_FACE('',(#1283),#1046,.T.);
#6000=ADVANCED_FACE('',(#1284,#610),#5691,.T.);
#6001=ADVANCED_FACE('',(#1285),#1047,.F.);
#6002=ADVANCED_FACE('',(#1286,#611),#5692,.T.);
#6003=ADVANCED_FACE('',(#1287),#1048,.T.);
#6004=ADVANCED_FACE('',(#1288,#612),#5693,.T.);
#6005=ADVANCED_FACE('',(#1289),#1049,.F.);
#6006=ADVANCED_FACE('',(#1290),#5694,.T.);
#6007=ADVANCED_FACE('',(#1291),#311,.T.);
#6008=ADVANCED_FACE('',(#1292),#1050,.T.);
#6009=ADVANCED_FACE('',(#1293),#312,.T.);
#6010=ADVANCED_FACE('',(#1294,#613),#5695,.T.);
#6011=ADVANCED_FACE('',(#1295),#313,.T.);
#6012=ADVANCED_FACE('',(#1296),#1051,.T.);
#6013=ADVANCED_FACE('',(#1297),#314,.T.);
#6014=ADVANCED_FACE('',(#1298),#5696,.T.);
#6015=ADVANCED_FACE('',(#1299),#5697,.F.);
#6016=ADVANCED_FACE('',(#1300),#5698,.F.);
#6017=ADVANCED_FACE('',(#1301),#5699,.F.);
#6018=ADVANCED_FACE('',(#1302),#5700,.F.);
#6019=ADVANCED_FACE('',(#1303),#5701,.F.);
#6020=ADVANCED_FACE('',(#1304),#5702,.F.);
#6021=ADVANCED_FACE('',(#1305),#5703,.F.);
#6022=ADVANCED_FACE('',(#1306),#5704,.F.);
#6023=ADVANCED_FACE('',(#1307),#5705,.F.);
#6024=ADVANCED_FACE('',(#1308),#5706,.F.);
#6025=ADVANCED_FACE('',(#1309),#5707,.F.);
#6026=ADVANCED_FACE('',(#1310),#5708,.F.);
#6027=ADVANCED_FACE('',(#1311),#5709,.F.);
#6028=ADVANCED_FACE('',(#1312,#614),#5710,.T.);
#6029=ADVANCED_FACE('',(#1313),#1052,.T.);
#6030=ADVANCED_FACE('',(#1314,#615),#5711,.T.);
#6031=ADVANCED_FACE('',(#1315),#1053,.T.);
#6032=ADVANCED_FACE('',(#1316,#616),#5712,.T.);
#6033=ADVANCED_FACE('',(#1317),#1054,.T.);
#6034=ADVANCED_FACE('',(#1318,#617),#5713,.T.);
#6035=ADVANCED_FACE('',(#1319),#1055,.T.);
#6036=ADVANCED_FACE('',(#1320,#618),#5714,.T.);
#6037=ADVANCED_FACE('',(#1321),#1056,.T.);
#6038=ADVANCED_FACE('',(#1322,#619),#5715,.T.);
#6039=ADVANCED_FACE('',(#1323,#620),#1057,.F.);
#6040=ADVANCED_FACE('',(#1324),#5716,.F.);
#6041=ADVANCED_FACE('',(#1325),#5717,.F.);
#6042=ADVANCED_FACE('',(#1326),#5718,.F.);
#6043=ADVANCED_FACE('',(#1327),#5719,.F.);
#6044=ADVANCED_FACE('',(#1328,#621),#5720,.T.);
#6045=ADVANCED_FACE('',(#1329,#622),#1058,.T.);
#6046=ADVANCED_FACE('',(#1330,#623),#5721,.T.);
#6047=ADVANCED_FACE('',(#1331,#624),#1059,.F.);
#6048=ADVANCED_FACE('',(#1332),#5722,.F.);
#6049=ADVANCED_FACE('',(#1333),#5723,.F.);
#6050=ADVANCED_FACE('',(#1334),#5724,.F.);
#6051=ADVANCED_FACE('',(#1335),#5725,.F.);
#6052=ADVANCED_FACE('',(#1336),#5726,.F.);
#6053=ADVANCED_FACE('',(#1337),#5727,.F.);
#6054=ADVANCED_FACE('',(#1338),#5728,.F.);
#6055=ADVANCED_FACE('',(#1339),#5729,.F.);
#6056=ADVANCED_FACE('',(#1340),#5730,.F.);
#6057=ADVANCED_FACE('',(#1341),#5731,.T.);
#6058=ADVANCED_FACE('',(#1342),#315,.T.);
#6059=ADVANCED_FACE('',(#1343),#1060,.T.);
#6060=ADVANCED_FACE('',(#1344),#316,.T.);
#6061=ADVANCED_FACE('',(#1345,#625),#5732,.T.);
#6062=ADVANCED_FACE('',(#1346),#317,.T.);
#6063=ADVANCED_FACE('',(#1347),#1061,.T.);
#6064=ADVANCED_FACE('',(#1348),#1062,.F.);
#6065=ADVANCED_FACE('',(#1349),#5733,.T.);
#6066=ADVANCED_FACE('',(#1350),#1063,.F.);
#6067=ADVANCED_FACE('',(#1351),#5734,.F.);
#6068=ADVANCED_FACE('',(#1352),#5735,.F.);
#6069=ADVANCED_FACE('',(#1353),#5736,.T.);
#6070=ADVANCED_FACE('',(#1354),#5737,.F.);
#6071=ADVANCED_FACE('',(#1355),#5738,.F.);
#6072=ADVANCED_FACE('',(#1356),#5739,.F.);
#6073=ADVANCED_FACE('',(#1357),#5740,.F.);
#6074=ADVANCED_FACE('',(#1358),#5741,.T.);
#6075=ADVANCED_FACE('',(#1359),#5742,.F.);
#6076=ADVANCED_FACE('',(#1360),#5743,.F.);
#6077=ADVANCED_FACE('',(#1361),#5744,.F.);
#6078=ADVANCED_FACE('',(#1362,#626,#627),#1064,.T.);
#6079=ADVANCED_FACE('',(#1363,#628),#5745,.T.);
#6080=ADVANCED_FACE('',(#1364,#629),#5746,.F.);
#6081=ADVANCED_FACE('',(#1365),#1065,.F.);
#6082=ADVANCED_FACE('',(#1366),#1066,.T.);
#6083=ADVANCED_FACE('',(#1367,#630),#5747,.T.);
#6084=ADVANCED_FACE('',(#1368,#631),#5748,.F.);
#6085=ADVANCED_FACE('',(#1369),#1067,.F.);
#6086=ADVANCED_FACE('',(#1370),#1068,.T.);
#6087=ADVANCED_FACE('',(#1371,#632),#5749,.T.);
#6088=ADVANCED_FACE('',(#1372,#633),#5750,.F.);
#6089=ADVANCED_FACE('',(#1373),#1069,.F.);
#6090=ADVANCED_FACE('',(#1374),#1070,.T.);
#6091=ADVANCED_FACE('',(#1375,#634),#5751,.T.);
#6092=ADVANCED_FACE('',(#1376,#635),#5752,.F.);
#6093=ADVANCED_FACE('',(#1377),#1071,.F.);
#6094=ADVANCED_FACE('',(#1378),#1072,.T.);
#6095=ADVANCED_FACE('',(#1379,#636),#5753,.T.);
#6096=ADVANCED_FACE('',(#1380,#637),#5754,.F.);
#6097=ADVANCED_FACE('',(#1381),#5755,.F.);
#6098=ADVANCED_FACE('',(#1382),#5756,.F.);
#6099=ADVANCED_FACE('',(#1383),#5757,.F.);
#6100=ADVANCED_FACE('',(#1384,#638),#5758,.T.);
#6101=ADVANCED_FACE('',(#1385),#1073,.F.);
#6102=ADVANCED_FACE('',(#1386),#1074,.T.);
#6103=ADVANCED_FACE('',(#1387),#1075,.T.);
#6104=ADVANCED_FACE('',(#1388,#639),#5759,.F.);
#6105=ADVANCED_FACE('',(#1389),#1076,.T.);
#6106=ADVANCED_FACE('',(#1390,#640),#5760,.T.);
#6107=ADVANCED_FACE('',(#1391,#641),#5761,.F.);
#6108=ADVANCED_FACE('',(#1392),#1077,.F.);
#6109=ADVANCED_FACE('',(#1393),#5762,.F.);
#6110=ADVANCED_FACE('',(#1394),#5763,.F.);
#6111=ADVANCED_FACE('',(#1395),#5764,.F.);
#6112=ADVANCED_FACE('',(#1396,#642),#5765,.T.);
#6113=ADVANCED_FACE('',(#1397),#1078,.F.);
#6114=ADVANCED_FACE('',(#1398),#1079,.T.);
#6115=ADVANCED_FACE('',(#1399,#643),#5766,.F.);
#6116=ADVANCED_FACE('',(#1400),#5767,.T.);
#6117=ADVANCED_FACE('',(#1401),#5768,.T.);
#6118=ADVANCED_FACE('',(#1402,#644),#5769,.T.);
#6119=ADVANCED_FACE('',(#1403,#645),#1080,.T.);
#6120=ADVANCED_FACE('',(#1404,#646),#5770,.F.);
#6121=ADVANCED_FACE('',(#1405),#1081,.F.);
#6122=ADVANCED_FACE('',(#1406),#5771,.F.);
#6123=ADVANCED_FACE('',(#1407),#1082,.T.);
#6124=ADVANCED_FACE('',(#1408),#5772,.T.);
#6125=ADVANCED_FACE('',(#1409,#647),#5773,.F.);
#6126=ADVANCED_FACE('',(#1410),#1083,.F.);
#6127=ADVANCED_FACE('',(#1411),#1084,.T.);
#6128=ADVANCED_FACE('',(#1412,#648),#5774,.T.);
#6129=ADVANCED_FACE('',(#1413,#649),#5775,.F.);
#6130=ADVANCED_FACE('',(#1414),#1085,.F.);
#6131=ADVANCED_FACE('',(#1415),#1086,.T.);
#6132=ADVANCED_FACE('',(#1416,#650),#5776,.T.);
#6133=ADVANCED_FACE('',(#1417,#651),#5777,.F.);
#6134=ADVANCED_FACE('',(#1418),#5778,.T.);
#6135=ADVANCED_FACE('',(#1419),#5779,.T.);
#6136=ADVANCED_FACE('',(#1420),#5780,.T.);
#6137=ADVANCED_FACE('',(#1421),#5781,.T.);
#6138=ADVANCED_FACE('',(#1422),#5782,.T.);
#6139=ADVANCED_FACE('',(#1423),#5783,.F.);
#6140=ADVANCED_FACE('',(#1424),#5784,.T.);
#6141=ADVANCED_FACE('',(#1425),#5785,.T.);
#6142=ADVANCED_FACE('',(#1426),#5786,.T.);
#6143=ADVANCED_FACE('',(#1427),#5787,.F.);
#6144=ADVANCED_FACE('',(#1428),#5788,.T.);
#6145=ADVANCED_FACE('',(#1429),#318,.T.);
#6146=ADVANCED_FACE('',(#1430),#1087,.T.);
#6147=ADVANCED_FACE('',(#1431),#319,.T.);
#6148=ADVANCED_FACE('',(#1432,#652),#5789,.T.);
#6149=ADVANCED_FACE('',(#1433),#320,.T.);
#6150=ADVANCED_FACE('',(#1434),#1088,.T.);
#6151=ADVANCED_FACE('',(#1435),#321,.T.);
#6152=ADVANCED_FACE('',(#1436),#5790,.T.);
#6153=ADVANCED_FACE('',(#1437),#5791,.F.);
#6154=ADVANCED_FACE('',(#1438),#5792,.F.);
#6155=ADVANCED_FACE('',(#1439),#5793,.F.);
#6156=ADVANCED_FACE('',(#1440),#5794,.F.);
#6157=ADVANCED_FACE('',(#1441),#5795,.F.);
#6158=ADVANCED_FACE('',(#1442),#5796,.F.);
#6159=ADVANCED_FACE('',(#1443),#5797,.F.);
#6160=ADVANCED_FACE('',(#1444),#5798,.F.);
#6161=ADVANCED_FACE('',(#1445),#1089,.F.);
#6162=ADVANCED_FACE('',(#1446),#5799,.T.);
#6163=ADVANCED_FACE('',(#1447),#5800,.T.);
#6164=ADVANCED_FACE('',(#1448),#5801,.T.);
#6165=ADVANCED_FACE('',(#1449),#5802,.T.);
#6166=ADVANCED_FACE('',(#1450,#653),#5803,.T.);
#6167=ADVANCED_FACE('',(#1451,#654),#5804,.F.);
#6168=ADVANCED_FACE('',(#1452,#655),#5805,.F.);
#6169=ADVANCED_FACE('',(#1453),#1090,.T.);
#6170=ADVANCED_FACE('',(#1454),#5806,.T.);
#6171=ADVANCED_FACE('',(#1455),#1091,.T.);
#6172=ADVANCED_FACE('',(#1456),#5807,.F.);
#6173=ADVANCED_FACE('',(#1457),#1092,.T.);
#6174=ADVANCED_FACE('',(#1458,#656),#5808,.F.);
#6175=ADVANCED_FACE('',(#1459),#1093,.F.);
#6176=ADVANCED_FACE('',(#1460),#1094,.T.);
#6177=ADVANCED_FACE('',(#1461,#657),#5809,.T.);
#6178=ADVANCED_FACE('',(#1462,#658),#5810,.F.);
#6179=CLOSED_SHELL('',(#5811,#5812,#5813,#5814,#5815,#5816,#5817,#5818,
#5819,#5820,#5821,#5822,#5823,#5824,#5825,#5826,#5827));
#6180=CLOSED_SHELL('',(#5828,#5829,#5830,#5831,#5832,#5833));
#6181=CLOSED_SHELL('',(#5834,#5835,#5836,#5837,#5838,#5839));
#6182=CLOSED_SHELL('',(#5840,#5841,#5842,#5843,#5844,#5845,#5846,#5847,
#5848,#5849,#5850,#5851,#5852,#5853,#5854,#5855,#5856));
#6183=CLOSED_SHELL('',(#5857,#5858,#5859,#5860,#5861,#5862,#5863,#5864,
#5865,#5866));
#6184=CLOSED_SHELL('',(#5867,#5868,#5869,#5870,#5871,#5872,#5873,#5874,
#5875,#5876));
#6185=CLOSED_SHELL('',(#5877,#5878,#5879,#5880,#5881,#5882,#5883,#5884,
#5885,#5886,#5887,#5888,#5889,#5890,#5891,#5892,#5893));
#6186=CLOSED_SHELL('',(#5894,#5895,#5896,#5897,#5898,#5899,#5900,#5901,
#5902,#5903));
#6187=CLOSED_SHELL('',(#5904,#5905,#5906,#5907,#5908,#5909,#5910,#5911,
#5912,#5913));
#6188=CLOSED_SHELL('',(#5914,#5915,#5916,#5917,#5918,#5919,#5920,#5921,
#5922,#5923,#5924,#5925,#5926,#5927,#5928,#5929,#5930,#5931,#5932,#5933,
#5934,#5935,#5936,#5937,#5938,#5939,#5940,#5941,#5942,#5943,#5944));
#6189=CLOSED_SHELL('',(#5945,#5946,#5947,#5948,#5949,#5950,#5951,#5952,
#5953,#5954));
#6190=CLOSED_SHELL('',(#5955,#5956,#5957));
#6191=CLOSED_SHELL('',(#5958,#5959,#5960,#5961,#5962,#5963,#5964,#5965));
#6192=CLOSED_SHELL('',(#5966,#5967,#5968,#5969,#5970,#5971,#5972,#5973));
#6193=CLOSED_SHELL('',(#5974));
#6194=CLOSED_SHELL('',(#5975));
#6195=CLOSED_SHELL('',(#5976));
#6196=CLOSED_SHELL('',(#5977));
#6197=CLOSED_SHELL('',(#5978));
#6198=CLOSED_SHELL('',(#5979));
#6199=CLOSED_SHELL('',(#5980));
#6200=CLOSED_SHELL('',(#5981,#5982,#5983,#5984,#5985,#5986,#5987,#5988,
#5989,#5990,#5991,#5992,#5993,#5994,#5995,#5996,#5997));
#6201=CLOSED_SHELL('',(#5998,#5999,#6000,#6001));
#6202=CLOSED_SHELL('',(#6002,#6003,#6004,#6005));
#6203=CLOSED_SHELL('',(#6006,#6007,#6008,#6009,#6010,#6011,#6012,#6013,
#6014));
#6204=CLOSED_SHELL('',(#6015,#6016,#6017,#6018,#6019,#6020,#6021,#6022));
#6205=CLOSED_SHELL('',(#6023,#6024,#6025,#6026,#6027,#6028,#6029,#6030,
#6031,#6032,#6033,#6034,#6035,#6036,#6037,#6038,#6039));
#6206=CLOSED_SHELL('',(#6040,#6041,#6042,#6043,#6044,#6045,#6046,#6047));
#6207=CLOSED_SHELL('',(#6048,#6049,#6050,#6051,#6052,#6053,#6054,#6055));
#6208=CLOSED_SHELL('',(#6056,#6057,#6058,#6059,#6060,#6061,#6062,#6063));
#6209=CLOSED_SHELL('',(#6064,#6065,#6066,#6067,#6068,#6069,#6070,#6071,
#6072,#6073,#6074,#6075,#6076,#6077,#6078,#6079,#6080));
#6210=CLOSED_SHELL('',(#6081,#6082,#6083,#6084));
#6211=CLOSED_SHELL('',(#6085,#6086,#6087,#6088));
#6212=CLOSED_SHELL('',(#6089,#6090,#6091,#6092));
#6213=CLOSED_SHELL('',(#6093,#6094,#6095,#6096));
#6214=CLOSED_SHELL('',(#6097,#6098,#6099,#6100,#6101,#6102,#6103,#6104,
#6105,#6106,#6107));
#6215=CLOSED_SHELL('',(#6108,#6109,#6110,#6111,#6112,#6113,#6114,#6115,
#6116,#6117,#6118,#6119,#6120));
#6216=CLOSED_SHELL('',(#6121,#6122,#6123,#6124,#6125));
#6217=CLOSED_SHELL('',(#6126,#6127,#6128,#6129));
#6218=CLOSED_SHELL('',(#6130,#6131,#6132,#6133));
#6219=CLOSED_SHELL('',(#6134,#6135,#6136,#6137,#6138,#6139,#6140,#6141,
#6142,#6143));
#6220=CLOSED_SHELL('',(#6144,#6145,#6146,#6147,#6148,#6149,#6150,#6151,
#6152));
#6221=CLOSED_SHELL('',(#6153,#6154,#6155,#6156,#6157,#6158,#6159,#6160));
#6222=CLOSED_SHELL('',(#6161,#6162,#6163,#6164,#6165,#6166,#6167));
#6223=CLOSED_SHELL('',(#6168,#6169,#6170,#6171,#6172,#6173,#6174));
#6224=CLOSED_SHELL('',(#6175,#6176,#6177,#6178));
#6225=DERIVED_UNIT_ELEMENT(#6297,1.);
#6226=DERIVED_UNIT_ELEMENT(#12898,-3.);
#6227=DERIVED_UNIT_ELEMENT(#6297,1.);
#6228=DERIVED_UNIT_ELEMENT(#12898,-3.);
#6229=DERIVED_UNIT_ELEMENT(#6297,1.);
#6230=DERIVED_UNIT_ELEMENT(#12898,-3.);
#6231=DERIVED_UNIT_ELEMENT(#6297,1.);
#6232=DERIVED_UNIT_ELEMENT(#12898,-3.);
#6233=DERIVED_UNIT_ELEMENT(#6297,1.);
#6234=DERIVED_UNIT_ELEMENT(#12898,-3.);
#6235=DERIVED_UNIT_ELEMENT(#6297,1.);
#6236=DERIVED_UNIT_ELEMENT(#12898,-3.);
#6237=DERIVED_UNIT_ELEMENT(#6297,1.);
#6238=DERIVED_UNIT_ELEMENT(#12898,-3.);
#6239=DERIVED_UNIT_ELEMENT(#6297,1.);
#6240=DERIVED_UNIT_ELEMENT(#12898,-3.);
#6241=DERIVED_UNIT_ELEMENT(#6297,1.);
#6242=DERIVED_UNIT_ELEMENT(#12898,-3.);
#6243=DERIVED_UNIT_ELEMENT(#6297,1.);
#6244=DERIVED_UNIT_ELEMENT(#12898,-3.);
#6245=DERIVED_UNIT_ELEMENT(#6297,1.);
#6246=DERIVED_UNIT_ELEMENT(#12898,-3.);
#6247=DERIVED_UNIT_ELEMENT(#6297,1.);
#6248=DERIVED_UNIT_ELEMENT(#12898,-3.);
#6249=DERIVED_UNIT_ELEMENT(#6297,1.);
#6250=DERIVED_UNIT_ELEMENT(#12898,-3.);
#6251=DERIVED_UNIT_ELEMENT(#6297,1.);
#6252=DERIVED_UNIT_ELEMENT(#12898,-3.);
#6253=DERIVED_UNIT_ELEMENT(#6297,1.);
#6254=DERIVED_UNIT_ELEMENT(#12898,-3.);
#6255=DERIVED_UNIT_ELEMENT(#6297,1.);
#6256=DERIVED_UNIT_ELEMENT(#12898,-3.);
#6257=DERIVED_UNIT_ELEMENT(#6297,1.);
#6258=DERIVED_UNIT_ELEMENT(#12898,-3.);
#6259=DERIVED_UNIT_ELEMENT(#6297,1.);
#6260=DERIVED_UNIT_ELEMENT(#12898,-3.);
#6261=DERIVED_UNIT_ELEMENT(#6297,1.);
#6262=DERIVED_UNIT_ELEMENT(#12898,-3.);
#6263=DERIVED_UNIT_ELEMENT(#6297,1.);
#6264=DERIVED_UNIT_ELEMENT(#12898,-3.);
#6265=DERIVED_UNIT_ELEMENT(#6297,1.);
#6266=DERIVED_UNIT_ELEMENT(#12898,-3.);
#6267=DERIVED_UNIT_ELEMENT(#6297,1.);
#6268=DERIVED_UNIT_ELEMENT(#12898,-3.);
#6269=DERIVED_UNIT_ELEMENT(#6297,1.);
#6270=DERIVED_UNIT_ELEMENT(#12898,-3.);
#6271=DERIVED_UNIT_ELEMENT(#6297,1.);
#6272=DERIVED_UNIT_ELEMENT(#12898,-3.);
#6273=DERIVED_UNIT_ELEMENT(#6297,1.);
#6274=DERIVED_UNIT_ELEMENT(#12898,-3.);
#6275=DERIVED_UNIT_ELEMENT(#6297,1.);
#6276=DERIVED_UNIT_ELEMENT(#12898,-3.);
#6277=DERIVED_UNIT_ELEMENT(#6297,1.);
#6278=DERIVED_UNIT_ELEMENT(#12898,-3.);
#6279=DERIVED_UNIT_ELEMENT(#6297,1.);
#6280=DERIVED_UNIT_ELEMENT(#12898,-3.);
#6281=DERIVED_UNIT_ELEMENT(#6297,1.);
#6282=DERIVED_UNIT_ELEMENT(#12898,-3.);
#6283=DERIVED_UNIT_ELEMENT(#6297,1.);
#6284=DERIVED_UNIT_ELEMENT(#12898,-3.);
#6285=DERIVED_UNIT_ELEMENT(#6297,1.);
#6286=DERIVED_UNIT_ELEMENT(#12898,-3.);
#6287=DERIVED_UNIT_ELEMENT(#6297,1.);
#6288=DERIVED_UNIT_ELEMENT(#12898,-3.);
#6289=DERIVED_UNIT_ELEMENT(#6297,1.);
#6290=DERIVED_UNIT_ELEMENT(#12898,-3.);
#6291=DERIVED_UNIT_ELEMENT(#6297,1.);
#6292=DERIVED_UNIT_ELEMENT(#12898,-3.);
#6293=DERIVED_UNIT_ELEMENT(#6297,1.);
#6294=DERIVED_UNIT_ELEMENT(#12898,-3.);
#6295=DERIVED_UNIT_ELEMENT(#6297,1.);
#6296=DERIVED_UNIT_ELEMENT(#12898,-3.);
#6297=(
MASS_UNIT()
NAMED_UNIT(*)
SI_UNIT(.KILO.,.GRAM.)
);
#6298=DERIVED_UNIT((#6225,#6226));
#6299=DERIVED_UNIT((#6227,#6228));
#6300=DERIVED_UNIT((#6229,#6230));
#6301=DERIVED_UNIT((#6231,#6232));
#6302=DERIVED_UNIT((#6233,#6234));
#6303=DERIVED_UNIT((#6235,#6236));
#6304=DERIVED_UNIT((#6237,#6238));
#6305=DERIVED_UNIT((#6239,#6240));
#6306=DERIVED_UNIT((#6241,#6242));
#6307=DERIVED_UNIT((#6243,#6244));
#6308=DERIVED_UNIT((#6245,#6246));
#6309=DERIVED_UNIT((#6247,#6248));
#6310=DERIVED_UNIT((#6249,#6250));
#6311=DERIVED_UNIT((#6251,#6252));
#6312=DERIVED_UNIT((#6253,#6254));
#6313=DERIVED_UNIT((#6255,#6256));
#6314=DERIVED_UNIT((#6257,#6258));
#6315=DERIVED_UNIT((#6259,#6260));
#6316=DERIVED_UNIT((#6261,#6262));
#6317=DERIVED_UNIT((#6263,#6264));
#6318=DERIVED_UNIT((#6265,#6266));
#6319=DERIVED_UNIT((#6267,#6268));
#6320=DERIVED_UNIT((#6269,#6270));
#6321=DERIVED_UNIT((#6271,#6272));
#6322=DERIVED_UNIT((#6273,#6274));
#6323=DERIVED_UNIT((#6275,#6276));
#6324=DERIVED_UNIT((#6277,#6278));
#6325=DERIVED_UNIT((#6279,#6280));
#6326=DERIVED_UNIT((#6281,#6282));
#6327=DERIVED_UNIT((#6283,#6284));
#6328=DERIVED_UNIT((#6285,#6286));
#6329=DERIVED_UNIT((#6287,#6288));
#6330=DERIVED_UNIT((#6289,#6290));
#6331=DERIVED_UNIT((#6291,#6292));
#6332=DERIVED_UNIT((#6293,#6294));
#6333=DERIVED_UNIT((#6295,#6296));
#6334=MEASURE_REPRESENTATION_ITEM('density measure',
POSITIVE_RATIO_MEASURE(7850.),#6298);
#6335=MEASURE_REPRESENTATION_ITEM('density measure',
POSITIVE_RATIO_MEASURE(7850.),#6299);
#6336=MEASURE_REPRESENTATION_ITEM('density measure',
POSITIVE_RATIO_MEASURE(7850.),#6300);
#6337=MEASURE_REPRESENTATION_ITEM('density measure',
POSITIVE_RATIO_MEASURE(7850.),#6301);
#6338=MEASURE_REPRESENTATION_ITEM('density measure',
POSITIVE_RATIO_MEASURE(7850.),#6302);
#6339=MEASURE_REPRESENTATION_ITEM('density measure',
POSITIVE_RATIO_MEASURE(7850.),#6303);
#6340=MEASURE_REPRESENTATION_ITEM('density measure',
POSITIVE_RATIO_MEASURE(7850.),#6304);
#6341=MEASURE_REPRESENTATION_ITEM('density measure',
POSITIVE_RATIO_MEASURE(7850.),#6305);
#6342=MEASURE_REPRESENTATION_ITEM('density measure',
POSITIVE_RATIO_MEASURE(7850.),#6306);
#6343=MEASURE_REPRESENTATION_ITEM('density measure',
POSITIVE_RATIO_MEASURE(7850.),#6307);
#6344=MEASURE_REPRESENTATION_ITEM('density measure',
POSITIVE_RATIO_MEASURE(7850.),#6308);
#6345=MEASURE_REPRESENTATION_ITEM('density measure',
POSITIVE_RATIO_MEASURE(7850.),#6309);
#6346=MEASURE_REPRESENTATION_ITEM('density measure',
POSITIVE_RATIO_MEASURE(7850.),#6310);
#6347=MEASURE_REPRESENTATION_ITEM('density measure',
POSITIVE_RATIO_MEASURE(7850.),#6311);
#6348=MEASURE_REPRESENTATION_ITEM('density measure',
POSITIVE_RATIO_MEASURE(7850.),#6312);
#6349=MEASURE_REPRESENTATION_ITEM('density measure',
POSITIVE_RATIO_MEASURE(7850.),#6313);
#6350=MEASURE_REPRESENTATION_ITEM('density measure',
POSITIVE_RATIO_MEASURE(7850.),#6314);
#6351=MEASURE_REPRESENTATION_ITEM('density measure',
POSITIVE_RATIO_MEASURE(7850.),#6315);
#6352=MEASURE_REPRESENTATION_ITEM('density measure',
POSITIVE_RATIO_MEASURE(7850.),#6316);
#6353=MEASURE_REPRESENTATION_ITEM('density measure',
POSITIVE_RATIO_MEASURE(7850.),#6317);
#6354=MEASURE_REPRESENTATION_ITEM('density measure',
POSITIVE_RATIO_MEASURE(7850.),#6318);
#6355=MEASURE_REPRESENTATION_ITEM('density measure',
POSITIVE_RATIO_MEASURE(7850.),#6319);
#6356=MEASURE_REPRESENTATION_ITEM('density measure',
POSITIVE_RATIO_MEASURE(7850.),#6320);
#6357=MEASURE_REPRESENTATION_ITEM('density measure',
POSITIVE_RATIO_MEASURE(7850.),#6321);
#6358=MEASURE_REPRESENTATION_ITEM('density measure',
POSITIVE_RATIO_MEASURE(7850.),#6322);
#6359=MEASURE_REPRESENTATION_ITEM('density measure',
POSITIVE_RATIO_MEASURE(7850.),#6323);
#6360=MEASURE_REPRESENTATION_ITEM('density measure',
POSITIVE_RATIO_MEASURE(7850.),#6324);
#6361=MEASURE_REPRESENTATION_ITEM('density measure',
POSITIVE_RATIO_MEASURE(7850.),#6325);
#6362=MEASURE_REPRESENTATION_ITEM('density measure',
POSITIVE_RATIO_MEASURE(7850.),#6326);
#6363=MEASURE_REPRESENTATION_ITEM('density measure',
POSITIVE_RATIO_MEASURE(7850.),#6327);
#6364=MEASURE_REPRESENTATION_ITEM('density measure',
POSITIVE_RATIO_MEASURE(7850.),#6328);
#6365=MEASURE_REPRESENTATION_ITEM('density measure',
POSITIVE_RATIO_MEASURE(7850.),#6329);
#6366=MEASURE_REPRESENTATION_ITEM('density measure',
POSITIVE_RATIO_MEASURE(7850.),#6330);
#6367=MEASURE_REPRESENTATION_ITEM('density measure',
POSITIVE_RATIO_MEASURE(7850.),#6331);
#6368=MEASURE_REPRESENTATION_ITEM('density measure',
POSITIVE_RATIO_MEASURE(7850.),#6332);
#6369=MEASURE_REPRESENTATION_ITEM('density measure',
POSITIVE_RATIO_MEASURE(7850.),#6333);
#6370=PROPERTY_DEFINITION_REPRESENTATION(#6550,#6442);
#6371=PROPERTY_DEFINITION_REPRESENTATION(#6551,#6443);
#6372=PROPERTY_DEFINITION_REPRESENTATION(#6552,#6444);
#6373=PROPERTY_DEFINITION_REPRESENTATION(#6553,#6445);
#6374=PROPERTY_DEFINITION_REPRESENTATION(#6554,#6446);
#6375=PROPERTY_DEFINITION_REPRESENTATION(#6555,#6447);
#6376=PROPERTY_DEFINITION_REPRESENTATION(#6556,#6448);
#6377=PROPERTY_DEFINITION_REPRESENTATION(#6557,#6449);
#6378=PROPERTY_DEFINITION_REPRESENTATION(#6558,#6450);
#6379=PROPERTY_DEFINITION_REPRESENTATION(#6559,#6451);
#6380=PROPERTY_DEFINITION_REPRESENTATION(#6560,#6452);
#6381=PROPERTY_DEFINITION_REPRESENTATION(#6561,#6453);
#6382=PROPERTY_DEFINITION_REPRESENTATION(#6562,#6454);
#6383=PROPERTY_DEFINITION_REPRESENTATION(#6563,#6455);
#6384=PROPERTY_DEFINITION_REPRESENTATION(#6564,#6456);
#6385=PROPERTY_DEFINITION_REPRESENTATION(#6565,#6457);
#6386=PROPERTY_DEFINITION_REPRESENTATION(#6566,#6458);
#6387=PROPERTY_DEFINITION_REPRESENTATION(#6567,#6459);
#6388=PROPERTY_DEFINITION_REPRESENTATION(#6568,#6460);
#6389=PROPERTY_DEFINITION_REPRESENTATION(#6569,#6461);
#6390=PROPERTY_DEFINITION_REPRESENTATION(#6570,#6462);
#6391=PROPERTY_DEFINITION_REPRESENTATION(#6571,#6463);
#6392=PROPERTY_DEFINITION_REPRESENTATION(#6572,#6464);
#6393=PROPERTY_DEFINITION_REPRESENTATION(#6573,#6465);
#6394=PROPERTY_DEFINITION_REPRESENTATION(#6574,#6466);
#6395=PROPERTY_DEFINITION_REPRESENTATION(#6575,#6467);
#6396=PROPERTY_DEFINITION_REPRESENTATION(#6576,#6468);
#6397=PROPERTY_DEFINITION_REPRESENTATION(#6577,#6469);
#6398=PROPERTY_DEFINITION_REPRESENTATION(#6578,#6470);
#6399=PROPERTY_DEFINITION_REPRESENTATION(#6579,#6471);
#6400=PROPERTY_DEFINITION_REPRESENTATION(#6580,#6472);
#6401=PROPERTY_DEFINITION_REPRESENTATION(#6581,#6473);
#6402=PROPERTY_DEFINITION_REPRESENTATION(#6582,#6474);
#6403=PROPERTY_DEFINITION_REPRESENTATION(#6583,#6475);
#6404=PROPERTY_DEFINITION_REPRESENTATION(#6584,#6476);
#6405=PROPERTY_DEFINITION_REPRESENTATION(#6585,#6477);
#6406=PROPERTY_DEFINITION_REPRESENTATION(#6586,#6478);
#6407=PROPERTY_DEFINITION_REPRESENTATION(#6587,#6479);
#6408=PROPERTY_DEFINITION_REPRESENTATION(#6588,#6480);
#6409=PROPERTY_DEFINITION_REPRESENTATION(#6589,#6481);
#6410=PROPERTY_DEFINITION_REPRESENTATION(#6590,#6482);
#6411=PROPERTY_DEFINITION_REPRESENTATION(#6591,#6483);
#6412=PROPERTY_DEFINITION_REPRESENTATION(#6592,#6484);
#6413=PROPERTY_DEFINITION_REPRESENTATION(#6593,#6485);
#6414=PROPERTY_DEFINITION_REPRESENTATION(#6594,#6486);
#6415=PROPERTY_DEFINITION_REPRESENTATION(#6595,#6487);
#6416=PROPERTY_DEFINITION_REPRESENTATION(#6596,#6488);
#6417=PROPERTY_DEFINITION_REPRESENTATION(#6597,#6489);
#6418=PROPERTY_DEFINITION_REPRESENTATION(#6598,#6490);
#6419=PROPERTY_DEFINITION_REPRESENTATION(#6599,#6491);
#6420=PROPERTY_DEFINITION_REPRESENTATION(#6600,#6492);
#6421=PROPERTY_DEFINITION_REPRESENTATION(#6601,#6493);
#6422=PROPERTY_DEFINITION_REPRESENTATION(#6602,#6494);
#6423=PROPERTY_DEFINITION_REPRESENTATION(#6603,#6495);
#6424=PROPERTY_DEFINITION_REPRESENTATION(#6604,#6496);
#6425=PROPERTY_DEFINITION_REPRESENTATION(#6605,#6497);
#6426=PROPERTY_DEFINITION_REPRESENTATION(#6606,#6498);
#6427=PROPERTY_DEFINITION_REPRESENTATION(#6607,#6499);
#6428=PROPERTY_DEFINITION_REPRESENTATION(#6608,#6500);
#6429=PROPERTY_DEFINITION_REPRESENTATION(#6609,#6501);
#6430=PROPERTY_DEFINITION_REPRESENTATION(#6610,#6502);
#6431=PROPERTY_DEFINITION_REPRESENTATION(#6611,#6503);
#6432=PROPERTY_DEFINITION_REPRESENTATION(#6612,#6504);
#6433=PROPERTY_DEFINITION_REPRESENTATION(#6613,#6505);
#6434=PROPERTY_DEFINITION_REPRESENTATION(#6614,#6506);
#6435=PROPERTY_DEFINITION_REPRESENTATION(#6615,#6507);
#6436=PROPERTY_DEFINITION_REPRESENTATION(#6616,#6508);
#6437=PROPERTY_DEFINITION_REPRESENTATION(#6617,#6509);
#6438=PROPERTY_DEFINITION_REPRESENTATION(#6618,#6510);
#6439=PROPERTY_DEFINITION_REPRESENTATION(#6619,#6511);
#6440=PROPERTY_DEFINITION_REPRESENTATION(#6620,#6512);
#6441=PROPERTY_DEFINITION_REPRESENTATION(#6621,#6513);
#6442=REPRESENTATION('material name',(#6514),#12856);
#6443=REPRESENTATION('density',(#6334),#12856);
#6444=REPRESENTATION('material name',(#6515),#12857);
#6445=REPRESENTATION('density',(#6335),#12857);
#6446=REPRESENTATION('material name',(#6516),#12858);
#6447=REPRESENTATION('density',(#6336),#12858);
#6448=REPRESENTATION('material name',(#6517),#12859);
#6449=REPRESENTATION('density',(#6337),#12859);
#6450=REPRESENTATION('material name',(#6518),#12860);
#6451=REPRESENTATION('density',(#6338),#12860);
#6452=REPRESENTATION('material name',(#6519),#12861);
#6453=REPRESENTATION('density',(#6339),#12861);
#6454=REPRESENTATION('material name',(#6520),#12862);
#6455=REPRESENTATION('density',(#6340),#12862);
#6456=REPRESENTATION('material name',(#6521),#12863);
#6457=REPRESENTATION('density',(#6341),#12863);
#6458=REPRESENTATION('material name',(#6522),#12864);
#6459=REPRESENTATION('density',(#6342),#12864);
#6460=REPRESENTATION('material name',(#6523),#12865);
#6461=REPRESENTATION('density',(#6343),#12865);
#6462=REPRESENTATION('material name',(#6524),#12866);
#6463=REPRESENTATION('density',(#6344),#12866);
#6464=REPRESENTATION('material name',(#6525),#12867);
#6465=REPRESENTATION('density',(#6345),#12867);
#6466=REPRESENTATION('material name',(#6526),#12869);
#6467=REPRESENTATION('density',(#6346),#12869);
#6468=REPRESENTATION('material name',(#6527),#12870);
#6469=REPRESENTATION('density',(#6347),#12870);
#6470=REPRESENTATION('material name',(#6528),#12871);
#6471=REPRESENTATION('density',(#6348),#12871);
#6472=REPRESENTATION('material name',(#6529),#12872);
#6473=REPRESENTATION('density',(#6349),#12872);
#6474=REPRESENTATION('material name',(#6530),#12873);
#6475=REPRESENTATION('density',(#6350),#12873);
#6476=REPRESENTATION('material name',(#6531),#12874);
#6477=REPRESENTATION('density',(#6351),#12874);
#6478=REPRESENTATION('material name',(#6532),#12876);
#6479=REPRESENTATION('density',(#6352),#12876);
#6480=REPRESENTATION('material name',(#6533),#12877);
#6481=REPRESENTATION('density',(#6353),#12877);
#6482=REPRESENTATION('material name',(#6534),#12878);
#6483=REPRESENTATION('density',(#6354),#12878);
#6484=REPRESENTATION('material name',(#6535),#12880);
#6485=REPRESENTATION('density',(#6355),#12880);
#6486=REPRESENTATION('material name',(#6536),#12881);
#6487=REPRESENTATION('density',(#6356),#12881);
#6488=REPRESENTATION('material name',(#6537),#12882);
#6489=REPRESENTATION('density',(#6357),#12882);
#6490=REPRESENTATION('material name',(#6538),#12883);
#6491=REPRESENTATION('density',(#6358),#12883);
#6492=REPRESENTATION('material name',(#6539),#12884);
#6493=REPRESENTATION('density',(#6359),#12884);
#6494=REPRESENTATION('material name',(#6540),#12885);
#6495=REPRESENTATION('density',(#6360),#12885);
#6496=REPRESENTATION('material name',(#6541),#12886);
#6497=REPRESENTATION('density',(#6361),#12886);
#6498=REPRESENTATION('material name',(#6542),#12887);
#6499=REPRESENTATION('density',(#6362),#12887);
#6500=REPRESENTATION('material name',(#6543),#12888);
#6501=REPRESENTATION('density',(#6363),#12888);
#6502=REPRESENTATION('material name',(#6544),#12889);
#6503=REPRESENTATION('density',(#6364),#12889);
#6504=REPRESENTATION('material name',(#6545),#12890);
#6505=REPRESENTATION('density',(#6365),#12890);
#6506=REPRESENTATION('material name',(#6546),#12891);
#6507=REPRESENTATION('density',(#6366),#12891);
#6508=REPRESENTATION('material name',(#6547),#12893);
#6509=REPRESENTATION('density',(#6367),#12893);
#6510=REPRESENTATION('material name',(#6548),#12894);
#6511=REPRESENTATION('density',(#6368),#12894);
#6512=REPRESENTATION('material name',(#6549),#12895);
#6513=REPRESENTATION('density',(#6369),#12895);
#6514=DESCRIPTIVE_REPRESENTATION_ITEM('Steel','Steel');
#6515=DESCRIPTIVE_REPRESENTATION_ITEM('Steel','Steel');
#6516=DESCRIPTIVE_REPRESENTATION_ITEM('Steel','Steel');
#6517=DESCRIPTIVE_REPRESENTATION_ITEM('Steel','Steel');
#6518=DESCRIPTIVE_REPRESENTATION_ITEM('Steel','Steel');
#6519=DESCRIPTIVE_REPRESENTATION_ITEM('Steel','Steel');
#6520=DESCRIPTIVE_REPRESENTATION_ITEM('Steel','Steel');
#6521=DESCRIPTIVE_REPRESENTATION_ITEM('Steel','Steel');
#6522=DESCRIPTIVE_REPRESENTATION_ITEM('Steel','Steel');
#6523=DESCRIPTIVE_REPRESENTATION_ITEM('Steel','Steel');
#6524=DESCRIPTIVE_REPRESENTATION_ITEM('Steel','Steel');
#6525=DESCRIPTIVE_REPRESENTATION_ITEM('Steel','Steel');
#6526=DESCRIPTIVE_REPRESENTATION_ITEM('Steel','Steel');
#6527=DESCRIPTIVE_REPRESENTATION_ITEM('Steel','Steel');
#6528=DESCRIPTIVE_REPRESENTATION_ITEM('Steel','Steel');
#6529=DESCRIPTIVE_REPRESENTATION_ITEM('Steel','Steel');
#6530=DESCRIPTIVE_REPRESENTATION_ITEM('Steel','Steel');
#6531=DESCRIPTIVE_REPRESENTATION_ITEM('Steel','Steel');
#6532=DESCRIPTIVE_REPRESENTATION_ITEM('Steel','Steel');
#6533=DESCRIPTIVE_REPRESENTATION_ITEM('Steel','Steel');
#6534=DESCRIPTIVE_REPRESENTATION_ITEM('Steel','Steel');
#6535=DESCRIPTIVE_REPRESENTATION_ITEM('Steel','Steel');
#6536=DESCRIPTIVE_REPRESENTATION_ITEM('Steel','Steel');
#6537=DESCRIPTIVE_REPRESENTATION_ITEM('Steel','Steel');
#6538=DESCRIPTIVE_REPRESENTATION_ITEM('Steel','Steel');
#6539=DESCRIPTIVE_REPRESENTATION_ITEM('Steel','Steel');
#6540=DESCRIPTIVE_REPRESENTATION_ITEM('Steel','Steel');
#6541=DESCRIPTIVE_REPRESENTATION_ITEM('Steel','Steel');
#6542=DESCRIPTIVE_REPRESENTATION_ITEM('Steel','Steel');
#6543=DESCRIPTIVE_REPRESENTATION_ITEM('Steel','Steel');
#6544=DESCRIPTIVE_REPRESENTATION_ITEM('Steel','Steel');
#6545=DESCRIPTIVE_REPRESENTATION_ITEM('Steel','Steel');
#6546=DESCRIPTIVE_REPRESENTATION_ITEM('Steel','Steel');
#6547=DESCRIPTIVE_REPRESENTATION_ITEM('Steel','Steel');
#6548=DESCRIPTIVE_REPRESENTATION_ITEM('Steel','Steel');
#6549=DESCRIPTIVE_REPRESENTATION_ITEM('Steel','Steel');
#6550=PROPERTY_DEFINITION('material property','material name',#13099);
#6551=PROPERTY_DEFINITION('material property','density of part',#13099);
#6552=PROPERTY_DEFINITION('material property','material name',#13100);
#6553=PROPERTY_DEFINITION('material property','density of part',#13100);
#6554=PROPERTY_DEFINITION('material property','material name',#13101);
#6555=PROPERTY_DEFINITION('material property','density of part',#13101);
#6556=PROPERTY_DEFINITION('material property','material name',#13102);
#6557=PROPERTY_DEFINITION('material property','density of part',#13102);
#6558=PROPERTY_DEFINITION('material property','material name',#13103);
#6559=PROPERTY_DEFINITION('material property','density of part',#13103);
#6560=PROPERTY_DEFINITION('material property','material name',#13104);
#6561=PROPERTY_DEFINITION('material property','density of part',#13104);
#6562=PROPERTY_DEFINITION('material property','material name',#13105);
#6563=PROPERTY_DEFINITION('material property','density of part',#13105);
#6564=PROPERTY_DEFINITION('material property','material name',#13106);
#6565=PROPERTY_DEFINITION('material property','density of part',#13106);
#6566=PROPERTY_DEFINITION('material property','material name',#13107);
#6567=PROPERTY_DEFINITION('material property','density of part',#13107);
#6568=PROPERTY_DEFINITION('material property','material name',#13108);
#6569=PROPERTY_DEFINITION('material property','density of part',#13108);
#6570=PROPERTY_DEFINITION('material property','material name',#13109);
#6571=PROPERTY_DEFINITION('material property','density of part',#13109);
#6572=PROPERTY_DEFINITION('material property','material name',#13110);
#6573=PROPERTY_DEFINITION('material property','density of part',#13110);
#6574=PROPERTY_DEFINITION('material property','material name',#13112);
#6575=PROPERTY_DEFINITION('material property','density of part',#13112);
#6576=PROPERTY_DEFINITION('material property','material name',#13113);
#6577=PROPERTY_DEFINITION('material property','density of part',#13113);
#6578=PROPERTY_DEFINITION('material property','material name',#13114);
#6579=PROPERTY_DEFINITION('material property','density of part',#13114);
#6580=PROPERTY_DEFINITION('material property','material name',#13115);
#6581=PROPERTY_DEFINITION('material property','density of part',#13115);
#6582=PROPERTY_DEFINITION('material property','material name',#13116);
#6583=PROPERTY_DEFINITION('material property','density of part',#13116);
#6584=PROPERTY_DEFINITION('material property','material name',#13117);
#6585=PROPERTY_DEFINITION('material property','density of part',#13117);
#6586=PROPERTY_DEFINITION('material property','material name',#13119);
#6587=PROPERTY_DEFINITION('material property','density of part',#13119);
#6588=PROPERTY_DEFINITION('material property','material name',#13120);
#6589=PROPERTY_DEFINITION('material property','density of part',#13120);
#6590=PROPERTY_DEFINITION('material property','material name',#13121);
#6591=PROPERTY_DEFINITION('material property','density of part',#13121);
#6592=PROPERTY_DEFINITION('material property','material name',#13123);
#6593=PROPERTY_DEFINITION('material property','density of part',#13123);
#6594=PROPERTY_DEFINITION('material property','material name',#13124);
#6595=PROPERTY_DEFINITION('material property','density of part',#13124);
#6596=PROPERTY_DEFINITION('material property','material name',#13125);
#6597=PROPERTY_DEFINITION('material property','density of part',#13125);
#6598=PROPERTY_DEFINITION('material property','material name',#13126);
#6599=PROPERTY_DEFINITION('material property','density of part',#13126);
#6600=PROPERTY_DEFINITION('material property','material name',#13127);
#6601=PROPERTY_DEFINITION('material property','density of part',#13127);
#6602=PROPERTY_DEFINITION('material property','material name',#13128);
#6603=PROPERTY_DEFINITION('material property','density of part',#13128);
#6604=PROPERTY_DEFINITION('material property','material name',#13129);
#6605=PROPERTY_DEFINITION('material property','density of part',#13129);
#6606=PROPERTY_DEFINITION('material property','material name',#13130);
#6607=PROPERTY_DEFINITION('material property','density of part',#13130);
#6608=PROPERTY_DEFINITION('material property','material name',#13131);
#6609=PROPERTY_DEFINITION('material property','density of part',#13131);
#6610=PROPERTY_DEFINITION('material property','material name',#13132);
#6611=PROPERTY_DEFINITION('material property','density of part',#13132);
#6612=PROPERTY_DEFINITION('material property','material name',#13133);
#6613=PROPERTY_DEFINITION('material property','density of part',#13133);
#6614=PROPERTY_DEFINITION('material property','material name',#13134);
#6615=PROPERTY_DEFINITION('material property','density of part',#13134);
#6616=PROPERTY_DEFINITION('material property','material name',#13136);
#6617=PROPERTY_DEFINITION('material property','density of part',#13136);
#6618=PROPERTY_DEFINITION('material property','material name',#13137);
#6619=PROPERTY_DEFINITION('material property','density of part',#13137);
#6620=PROPERTY_DEFINITION('material property','material name',#13138);
#6621=PROPERTY_DEFINITION('material property','density of part',#13138);
#6622=AXIS2_PLACEMENT_3D('',#9420,#7414,#7415);
#6623=AXIS2_PLACEMENT_3D('',#9421,#7416,#7417);
#6624=AXIS2_PLACEMENT_3D('',#9422,#7418,#7419);
#6625=AXIS2_PLACEMENT_3D('',#9423,#7420,#7421);
#6626=AXIS2_PLACEMENT_3D('',#9432,#7426,#7427);
#6627=AXIS2_PLACEMENT_3D('',#9438,#7431,#7432);
#6628=AXIS2_PLACEMENT_3D('',#9444,#7436,#7437);
#6629=AXIS2_PLACEMENT_3D('',#9447,#7440,#7441);
#6630=AXIS2_PLACEMENT_3D('',#9448,#7442,#7443);
#6631=AXIS2_PLACEMENT_3D('',#9450,#7444,#7445);
#6632=AXIS2_PLACEMENT_3D('',#9453,#7447,#7448);
#6633=AXIS2_PLACEMENT_3D('',#9454,#7449,#7450);
#6634=AXIS2_PLACEMENT_3D('',#9456,#7451,#7452);
#6635=AXIS2_PLACEMENT_3D('',#9459,#7454,#7455);
#6636=AXIS2_PLACEMENT_3D('',#9460,#7456,#7457);
#6637=AXIS2_PLACEMENT_3D('',#9462,#7458,#7459);
#6638=AXIS2_PLACEMENT_3D('',#9465,#7461,#7462);
#6639=AXIS2_PLACEMENT_3D('',#9466,#7463,#7464);
#6640=AXIS2_PLACEMENT_3D('',#9468,#7465,#7466);
#6641=AXIS2_PLACEMENT_3D('',#9471,#7468,#7469);
#6642=AXIS2_PLACEMENT_3D('',#9472,#7470,#7471);
#6643=AXIS2_PLACEMENT_3D('',#9474,#7472,#7473);
#6644=AXIS2_PLACEMENT_3D('',#9477,#7475,#7476);
#6645=AXIS2_PLACEMENT_3D('',#9478,#7477,#7478);
#6646=AXIS2_PLACEMENT_3D('',#9480,#7479,#7480);
#6647=AXIS2_PLACEMENT_3D('',#9483,#7482,#7483);
#6648=AXIS2_PLACEMENT_3D('',#9484,#7484,#7485);
#6649=AXIS2_PLACEMENT_3D('',#9493,#7490,#7491);
#6650=AXIS2_PLACEMENT_3D('',#9499,#7495,#7496);
#6651=AXIS2_PLACEMENT_3D('',#9505,#7500,#7501);
#6652=AXIS2_PLACEMENT_3D('',#9508,#7504,#7505);
#6653=AXIS2_PLACEMENT_3D('',#9509,#7506,#7507);
#6654=AXIS2_PLACEMENT_3D('',#9510,#7508,#7509);
#6655=AXIS2_PLACEMENT_3D('',#9511,#7510,#7511);
#6656=AXIS2_PLACEMENT_3D('',#9520,#7516,#7517);
#6657=AXIS2_PLACEMENT_3D('',#9526,#7521,#7522);
#6658=AXIS2_PLACEMENT_3D('',#9532,#7526,#7527);
#6659=AXIS2_PLACEMENT_3D('',#9535,#7530,#7531);
#6660=AXIS2_PLACEMENT_3D('',#9536,#7532,#7533);
#6661=AXIS2_PLACEMENT_3D('',#9537,#7534,#7535);
#6662=AXIS2_PLACEMENT_3D('',#9538,#7536,#7537);
#6663=AXIS2_PLACEMENT_3D('',#9547,#7542,#7543);
#6664=AXIS2_PLACEMENT_3D('',#9553,#7547,#7548);
#6665=AXIS2_PLACEMENT_3D('',#9559,#7552,#7553);
#6666=AXIS2_PLACEMENT_3D('',#9562,#7556,#7557);
#6667=AXIS2_PLACEMENT_3D('',#9563,#7558,#7559);
#6668=AXIS2_PLACEMENT_3D('',#9564,#7560,#7561);
#6669=AXIS2_PLACEMENT_3D('',#9565,#7562,#7563);
#6670=AXIS2_PLACEMENT_3D('',#9567,#7564,#7565);
#6671=AXIS2_PLACEMENT_3D('',#9570,#7567,#7568);
#6672=AXIS2_PLACEMENT_3D('',#9571,#7569,#7570);
#6673=AXIS2_PLACEMENT_3D('',#9573,#7571,#7572);
#6674=AXIS2_PLACEMENT_3D('',#9576,#7574,#7575);
#6675=AXIS2_PLACEMENT_3D('',#9577,#7576,#7577);
#6676=AXIS2_PLACEMENT_3D('',#9579,#7578,#7579);
#6677=AXIS2_PLACEMENT_3D('',#9582,#7581,#7582);
#6678=AXIS2_PLACEMENT_3D('',#9583,#7583,#7584);
#6679=AXIS2_PLACEMENT_3D('',#9585,#7585,#7586);
#6680=AXIS2_PLACEMENT_3D('',#9588,#7588,#7589);
#6681=AXIS2_PLACEMENT_3D('',#9589,#7590,#7591);
#6682=AXIS2_PLACEMENT_3D('',#9591,#7592,#7593);
#6683=AXIS2_PLACEMENT_3D('',#9594,#7595,#7596);
#6684=AXIS2_PLACEMENT_3D('',#9595,#7597,#7598);
#6685=AXIS2_PLACEMENT_3D('',#9597,#7599,#7600);
#6686=AXIS2_PLACEMENT_3D('',#9600,#7602,#7603);
#6687=AXIS2_PLACEMENT_3D('',#9601,#7604,#7605);
#6688=AXIS2_PLACEMENT_3D('',#9603,#7606,#7607);
#6689=AXIS2_PLACEMENT_3D('',#9606,#7609,#7610);
#6690=AXIS2_PLACEMENT_3D('',#9607,#7611,#7612);
#6691=AXIS2_PLACEMENT_3D('',#9616,#7617,#7618);
#6692=AXIS2_PLACEMENT_3D('',#9625,#7623,#7624);
#6693=AXIS2_PLACEMENT_3D('',#9631,#7628,#7629);
#6694=AXIS2_PLACEMENT_3D('',#9637,#7633,#7634);
#6695=AXIS2_PLACEMENT_3D('',#9644,#7639,#7640);
#6696=AXIS2_PLACEMENT_3D('',#9648,#7643,#7644);
#6697=AXIS2_PLACEMENT_3D('',#9653,#7648,#7649);
#6698=AXIS2_PLACEMENT_3D('',#9655,#7651,#7652);
#6699=AXIS2_PLACEMENT_3D('',#9656,#7653,#7654);
#6700=AXIS2_PLACEMENT_3D('',#9657,#7655,#7656);
#6701=AXIS2_PLACEMENT_3D('',#9658,#7657,#7658);
#6702=AXIS2_PLACEMENT_3D('',#9660,#7659,#7660);
#6703=AXIS2_PLACEMENT_3D('',#9663,#7662,#7663);
#6704=AXIS2_PLACEMENT_3D('',#9664,#7664,#7665);
#6705=AXIS2_PLACEMENT_3D('',#9666,#7666,#7667);
#6706=AXIS2_PLACEMENT_3D('',#9669,#7669,#7670);
#6707=AXIS2_PLACEMENT_3D('',#9670,#7671,#7672);
#6708=AXIS2_PLACEMENT_3D('',#9672,#7673,#7674);
#6709=AXIS2_PLACEMENT_3D('',#9675,#7676,#7677);
#6710=AXIS2_PLACEMENT_3D('',#9676,#7678,#7679);
#6711=AXIS2_PLACEMENT_3D('',#9678,#7680,#7681);
#6712=AXIS2_PLACEMENT_3D('',#9681,#7683,#7684);
#6713=AXIS2_PLACEMENT_3D('',#9682,#7685,#7686);
#6714=AXIS2_PLACEMENT_3D('',#9684,#7687,#7688);
#6715=AXIS2_PLACEMENT_3D('',#9687,#7690,#7691);
#6716=AXIS2_PLACEMENT_3D('',#9688,#7692,#7693);
#6717=AXIS2_PLACEMENT_3D('',#9690,#7694,#7695);
#6718=AXIS2_PLACEMENT_3D('',#9691,#7696,#7697);
#6719=AXIS2_PLACEMENT_3D('',#9694,#7699,#7700);
#6720=AXIS2_PLACEMENT_3D('',#9695,#7701,#7702);
#6721=AXIS2_PLACEMENT_3D('',#9697,#7703,#7704);
#6722=AXIS2_PLACEMENT_3D('',#9700,#7706,#7707);
#6723=AXIS2_PLACEMENT_3D('',#9701,#7708,#7709);
#6724=AXIS2_PLACEMENT_3D('',#9702,#7710,#7711);
#6725=AXIS2_PLACEMENT_3D('',#9703,#7712,#7713);
#6726=AXIS2_PLACEMENT_3D('',#9704,#7714,#7715);
#6727=AXIS2_PLACEMENT_3D('',#9706,#7716,#7717);
#6728=AXIS2_PLACEMENT_3D('',#9709,#7719,#7720);
#6729=AXIS2_PLACEMENT_3D('',#9710,#7721,#7722);
#6730=AXIS2_PLACEMENT_3D('',#9712,#7723,#7724);
#6731=AXIS2_PLACEMENT_3D('',#9715,#7726,#7727);
#6732=AXIS2_PLACEMENT_3D('',#9716,#7728,#7729);
#6733=AXIS2_PLACEMENT_3D('',#9718,#7730,#7731);
#6734=AXIS2_PLACEMENT_3D('',#9721,#7733,#7734);
#6735=AXIS2_PLACEMENT_3D('',#9722,#7735,#7736);
#6736=AXIS2_PLACEMENT_3D('',#9724,#7737,#7738);
#6737=AXIS2_PLACEMENT_3D('',#9727,#7740,#7741);
#6738=AXIS2_PLACEMENT_3D('',#9728,#7742,#7743);
#6739=AXIS2_PLACEMENT_3D('',#9730,#7744,#7745);
#6740=AXIS2_PLACEMENT_3D('',#9733,#7747,#7748);
#6741=AXIS2_PLACEMENT_3D('',#9734,#7749,#7750);
#6742=AXIS2_PLACEMENT_3D('',#9736,#7751,#7752);
#6743=AXIS2_PLACEMENT_3D('',#9737,#7753,#7754);
#6744=AXIS2_PLACEMENT_3D('',#9739,#7755,#7756);
#6745=AXIS2_PLACEMENT_3D('',#9741,#7758,#7759);
#6746=AXIS2_PLACEMENT_3D('',#9743,#7760,#7761);
#6747=AXIS2_PLACEMENT_3D('',#9746,#7763,#7764);
#6748=AXIS2_PLACEMENT_3D('',#9747,#7765,#7766);
#6749=AXIS2_PLACEMENT_3D('',#9748,#7767,#7768);
#6750=AXIS2_PLACEMENT_3D('',#9749,#7769,#7770);
#6751=AXIS2_PLACEMENT_3D('',#9750,#7771,#7772);
#6752=AXIS2_PLACEMENT_3D('',#9752,#7773,#7774);
#6753=AXIS2_PLACEMENT_3D('',#9755,#7776,#7777);
#6754=AXIS2_PLACEMENT_3D('',#9756,#7778,#7779);
#6755=AXIS2_PLACEMENT_3D('',#9758,#7780,#7781);
#6756=AXIS2_PLACEMENT_3D('',#9761,#7783,#7784);
#6757=AXIS2_PLACEMENT_3D('',#9762,#7785,#7786);
#6758=AXIS2_PLACEMENT_3D('',#9764,#7787,#7788);
#6759=AXIS2_PLACEMENT_3D('',#9767,#7790,#7791);
#6760=AXIS2_PLACEMENT_3D('',#9768,#7792,#7793);
#6761=AXIS2_PLACEMENT_3D('',#9770,#7794,#7795);
#6762=AXIS2_PLACEMENT_3D('',#9773,#7797,#7798);
#6763=AXIS2_PLACEMENT_3D('',#9774,#7799,#7800);
#6764=AXIS2_PLACEMENT_3D('',#9776,#7801,#7802);
#6765=AXIS2_PLACEMENT_3D('',#9779,#7804,#7805);
#6766=AXIS2_PLACEMENT_3D('',#9780,#7806,#7807);
#6767=AXIS2_PLACEMENT_3D('',#9782,#7808,#7809);
#6768=AXIS2_PLACEMENT_3D('',#9785,#7811,#7812);
#6769=AXIS2_PLACEMENT_3D('',#9786,#7813,#7814);
#6770=AXIS2_PLACEMENT_3D('',#9788,#7815,#7816);
#6771=AXIS2_PLACEMENT_3D('',#9791,#7818,#7819);
#6772=AXIS2_PLACEMENT_3D('',#9792,#7820,#7821);
#6773=AXIS2_PLACEMENT_3D('',#9801,#7826,#7827);
#6774=AXIS2_PLACEMENT_3D('',#9810,#7832,#7833);
#6775=AXIS2_PLACEMENT_3D('',#9816,#7837,#7838);
#6776=AXIS2_PLACEMENT_3D('',#9822,#7842,#7843);
#6777=AXIS2_PLACEMENT_3D('',#9829,#7848,#7849);
#6778=AXIS2_PLACEMENT_3D('',#9833,#7852,#7853);
#6779=AXIS2_PLACEMENT_3D('',#9838,#7857,#7858);
#6780=AXIS2_PLACEMENT_3D('',#9840,#7860,#7861);
#6781=AXIS2_PLACEMENT_3D('',#9841,#7862,#7863);
#6782=AXIS2_PLACEMENT_3D('',#9842,#7864,#7865);
#6783=AXIS2_PLACEMENT_3D('',#9843,#7866,#7867);
#6784=AXIS2_PLACEMENT_3D('',#9845,#7868,#7869);
#6785=AXIS2_PLACEMENT_3D('',#9848,#7871,#7872);
#6786=AXIS2_PLACEMENT_3D('',#9849,#7873,#7874);
#6787=AXIS2_PLACEMENT_3D('',#9851,#7875,#7876);
#6788=AXIS2_PLACEMENT_3D('',#9854,#7878,#7879);
#6789=AXIS2_PLACEMENT_3D('',#9855,#7880,#7881);
#6790=AXIS2_PLACEMENT_3D('',#9857,#7882,#7883);
#6791=AXIS2_PLACEMENT_3D('',#9860,#7885,#7886);
#6792=AXIS2_PLACEMENT_3D('',#9861,#7887,#7888);
#6793=AXIS2_PLACEMENT_3D('',#9863,#7889,#7890);
#6794=AXIS2_PLACEMENT_3D('',#9866,#7892,#7893);
#6795=AXIS2_PLACEMENT_3D('',#9867,#7894,#7895);
#6796=AXIS2_PLACEMENT_3D('',#9869,#7896,#7897);
#6797=AXIS2_PLACEMENT_3D('',#9872,#7899,#7900);
#6798=AXIS2_PLACEMENT_3D('',#9873,#7901,#7902);
#6799=AXIS2_PLACEMENT_3D('',#9875,#7903,#7904);
#6800=AXIS2_PLACEMENT_3D('',#9876,#7905,#7906);
#6801=AXIS2_PLACEMENT_3D('',#9879,#7908,#7909);
#6802=AXIS2_PLACEMENT_3D('',#9880,#7910,#7911);
#6803=AXIS2_PLACEMENT_3D('',#9882,#7912,#7913);
#6804=AXIS2_PLACEMENT_3D('',#9885,#7915,#7916);
#6805=AXIS2_PLACEMENT_3D('',#9886,#7917,#7918);
#6806=AXIS2_PLACEMENT_3D('',#9887,#7919,#7920);
#6807=AXIS2_PLACEMENT_3D('',#9888,#7921,#7922);
#6808=AXIS2_PLACEMENT_3D('',#9889,#7923,#7924);
#6809=AXIS2_PLACEMENT_3D('',#9891,#7925,#7926);
#6810=AXIS2_PLACEMENT_3D('',#9894,#7928,#7929);
#6811=AXIS2_PLACEMENT_3D('',#9895,#7930,#7931);
#6812=AXIS2_PLACEMENT_3D('',#9897,#7932,#7933);
#6813=AXIS2_PLACEMENT_3D('',#9900,#7935,#7936);
#6814=AXIS2_PLACEMENT_3D('',#9901,#7937,#7938);
#6815=AXIS2_PLACEMENT_3D('',#9903,#7939,#7940);
#6816=AXIS2_PLACEMENT_3D('',#9906,#7942,#7943);
#6817=AXIS2_PLACEMENT_3D('',#9907,#7944,#7945);
#6818=AXIS2_PLACEMENT_3D('',#9909,#7946,#7947);
#6819=AXIS2_PLACEMENT_3D('',#9912,#7949,#7950);
#6820=AXIS2_PLACEMENT_3D('',#9913,#7951,#7952);
#6821=AXIS2_PLACEMENT_3D('',#9915,#7953,#7954);
#6822=AXIS2_PLACEMENT_3D('',#9918,#7956,#7957);
#6823=AXIS2_PLACEMENT_3D('',#9919,#7958,#7959);
#6824=AXIS2_PLACEMENT_3D('',#9921,#7960,#7961);
#6825=AXIS2_PLACEMENT_3D('',#9922,#7962,#7963);
#6826=AXIS2_PLACEMENT_3D('',#9924,#7964,#7965);
#6827=AXIS2_PLACEMENT_3D('',#9926,#7967,#7968);
#6828=AXIS2_PLACEMENT_3D('',#9928,#7969,#7970);
#6829=AXIS2_PLACEMENT_3D('',#9931,#7972,#7973);
#6830=AXIS2_PLACEMENT_3D('',#9932,#7974,#7975);
#6831=AXIS2_PLACEMENT_3D('',#9933,#7976,#7977);
#6832=AXIS2_PLACEMENT_3D('',#9934,#7978,#7979);
#6833=AXIS2_PLACEMENT_3D('',#9935,#7980,#7981);
#6834=AXIS2_PLACEMENT_3D('',#9937,#7982,#7983);
#6835=AXIS2_PLACEMENT_3D('',#9940,#7985,#7986);
#6836=AXIS2_PLACEMENT_3D('',#9941,#7987,#7988);
#6837=AXIS2_PLACEMENT_3D('',#9942,#7989,#7990);
#6838=AXIS2_PLACEMENT_3D('',#9944,#7991,#7992);
#6839=AXIS2_PLACEMENT_3D('',#9947,#7994,#7995);
#6840=AXIS2_PLACEMENT_3D('',#9948,#7996,#7997);
#6841=AXIS2_PLACEMENT_3D('',#9949,#7998,#7999);
#6842=AXIS2_PLACEMENT_3D('',#9951,#8000,#8001);
#6843=AXIS2_PLACEMENT_3D('',#9954,#8003,#8004);
#6844=AXIS2_PLACEMENT_3D('',#9955,#8005,#8006);
#6845=AXIS2_PLACEMENT_3D('',#9956,#8007,#8008);
#6846=AXIS2_PLACEMENT_3D('',#9958,#8009,#8010);
#6847=AXIS2_PLACEMENT_3D('',#9961,#8012,#8013);
#6848=AXIS2_PLACEMENT_3D('',#9962,#8014,#8015);
#6849=AXIS2_PLACEMENT_3D('',#9963,#8016,#8017);
#6850=AXIS2_PLACEMENT_3D('',#9965,#8018,#8019);
#6851=AXIS2_PLACEMENT_3D('',#9968,#8021,#8022);
#6852=AXIS2_PLACEMENT_3D('',#9969,#8023,#8024);
#6853=AXIS2_PLACEMENT_3D('',#9971,#8025,#8026);
#6854=AXIS2_PLACEMENT_3D('',#9972,#8027,#8028);
#6855=AXIS2_PLACEMENT_3D('',#9974,#8029,#8030);
#6856=AXIS2_PLACEMENT_3D('',#9976,#8032,#8033);
#6857=AXIS2_PLACEMENT_3D('',#9978,#8034,#8035);
#6858=AXIS2_PLACEMENT_3D('',#9981,#8037,#8038);
#6859=AXIS2_PLACEMENT_3D('',#9982,#8039,#8040);
#6860=AXIS2_PLACEMENT_3D('',#9984,#8041,#8042);
#6861=AXIS2_PLACEMENT_3D('',#9985,#8043,#8044);
#6862=AXIS2_PLACEMENT_3D('',#9987,#8045,#8046);
#6863=AXIS2_PLACEMENT_3D('',#9989,#8048,#8049);
#6864=AXIS2_PLACEMENT_3D('',#9991,#8050,#8051);
#6865=AXIS2_PLACEMENT_3D('',#9994,#8053,#8054);
#6866=AXIS2_PLACEMENT_3D('',#9995,#8055,#8056);
#6867=AXIS2_PLACEMENT_3D('',#9997,#8057,#8058);
#6868=AXIS2_PLACEMENT_3D('',#9998,#8059,#8060);
#6869=AXIS2_PLACEMENT_3D('',#10000,#8061,#8062);
#6870=AXIS2_PLACEMENT_3D('',#10002,#8064,#8065);
#6871=AXIS2_PLACEMENT_3D('',#10027,#8078,#8079);
#6872=AXIS2_PLACEMENT_3D('',#10033,#8083,#8084);
#6873=AXIS2_PLACEMENT_3D('',#10039,#8088,#8089);
#6874=AXIS2_PLACEMENT_3D('',#10045,#8093,#8094);
#6875=AXIS2_PLACEMENT_3D('',#10049,#8097,#8098);
#6876=AXIS2_PLACEMENT_3D('',#10053,#8101,#8102);
#6877=AXIS2_PLACEMENT_3D('',#10056,#8105,#8106);
#6878=AXIS2_PLACEMENT_3D('',#10057,#8107,#8108);
#6879=AXIS2_PLACEMENT_3D('',#10063,#8112,#8113);
#6880=AXIS2_PLACEMENT_3D('',#10067,#8116,#8117);
#6881=AXIS2_PLACEMENT_3D('',#10071,#8120,#8121);
#6882=AXIS2_PLACEMENT_3D('',#10074,#8124,#8125);
#6883=AXIS2_PLACEMENT_3D('',#10075,#8126,#8127);
#6884=AXIS2_PLACEMENT_3D('',#10076,#8128,#8129);
#6885=AXIS2_PLACEMENT_3D('',#10077,#8130,#8131);
#6886=AXIS2_PLACEMENT_3D('',#10079,#8132,#8133);
#6887=AXIS2_PLACEMENT_3D('',#10082,#8135,#8136);
#6888=AXIS2_PLACEMENT_3D('',#10083,#8137,#8138);
#6889=AXIS2_PLACEMENT_3D('',#10085,#8139,#8140);
#6890=AXIS2_PLACEMENT_3D('',#10088,#8142,#8143);
#6891=AXIS2_PLACEMENT_3D('',#10089,#8144,#8145);
#6892=AXIS2_PLACEMENT_3D('',#10091,#8146,#8147);
#6893=AXIS2_PLACEMENT_3D('',#10094,#8149,#8150);
#6894=AXIS2_PLACEMENT_3D('',#10095,#8151,#8152);
#6895=AXIS2_PLACEMENT_3D('',#10097,#8153,#8154);
#6896=AXIS2_PLACEMENT_3D('',#10100,#8156,#8157);
#6897=AXIS2_PLACEMENT_3D('',#10101,#8158,#8159);
#6898=AXIS2_PLACEMENT_3D('',#10103,#8160,#8161);
#6899=AXIS2_PLACEMENT_3D('',#10106,#8163,#8164);
#6900=AXIS2_PLACEMENT_3D('',#10107,#8165,#8166);
#6901=AXIS2_PLACEMENT_3D('',#10109,#8167,#8168);
#6902=AXIS2_PLACEMENT_3D('',#10110,#8169,#8170);
#6903=AXIS2_PLACEMENT_3D('',#10112,#8171,#8172);
#6904=AXIS2_PLACEMENT_3D('',#10114,#8174,#8175);
#6905=AXIS2_PLACEMENT_3D('',#10116,#8176,#8177);
#6906=AXIS2_PLACEMENT_3D('',#10119,#8179,#8180);
#6907=AXIS2_PLACEMENT_3D('',#10120,#8181,#8182);
#6908=AXIS2_PLACEMENT_3D('',#10121,#8183,#8184);
#6909=AXIS2_PLACEMENT_3D('',#10122,#8185,#8186);
#6910=AXIS2_PLACEMENT_3D('',#11364,#8187,#8188);
#6911=AXIS2_PLACEMENT_3D('',#11490,#8189,#8190);
#6912=AXIS2_PLACEMENT_3D('',#11491,#8191,#8192);
#6913=AXIS2_PLACEMENT_3D('',#11492,#8193,#8194);
#6914=AXIS2_PLACEMENT_3D('',#11493,#8195,#8196);
#6915=AXIS2_PLACEMENT_3D('',#11494,#8197,#8198);
#6916=AXIS2_PLACEMENT_3D('',#11495,#8199,#8200);
#6917=AXIS2_PLACEMENT_3D('',#11498,#8201,#8202);
#6918=AXIS2_PLACEMENT_3D('',#11499,#8203,#8204);
#6919=AXIS2_PLACEMENT_3D('',#11501,#8205,#8206);
#6920=AXIS2_PLACEMENT_3D('',#11503,#8207,#8208);
#6921=AXIS2_PLACEMENT_3D('',#11504,#8209,#8210);
#6922=AXIS2_PLACEMENT_3D('',#11505,#8211,#8212);
#6923=AXIS2_PLACEMENT_3D('',#11508,#8214,#8215);
#6924=AXIS2_PLACEMENT_3D('',#11509,#8216,#8217);
#6925=AXIS2_PLACEMENT_3D('',#11511,#8218,#8219);
#6926=AXIS2_PLACEMENT_3D('',#11514,#8221,#8222);
#6927=AXIS2_PLACEMENT_3D('',#11515,#8223,#8224);
#6928=AXIS2_PLACEMENT_3D('',#11518,#8226,#8227);
#6929=AXIS2_PLACEMENT_3D('',#11519,#8228,#8229);
#6930=AXIS2_PLACEMENT_3D('',#11520,#8230,#8231);
#6931=AXIS2_PLACEMENT_3D('',#11522,#8232,#8233);
#6932=AXIS2_PLACEMENT_3D('',#11524,#8235,#8236);
#6933=AXIS2_PLACEMENT_3D('',#11526,#8237,#8238);
#6934=AXIS2_PLACEMENT_3D('',#11527,#8239,#8240);
#6935=AXIS2_PLACEMENT_3D('',#11529,#8242,#8243);
#6936=AXIS2_PLACEMENT_3D('',#11530,#8244,#8245);
#6937=AXIS2_PLACEMENT_3D('',#11533,#8246,#8247);
#6938=AXIS2_PLACEMENT_3D('',#11534,#8248,#8249);
#6939=AXIS2_PLACEMENT_3D('',#11536,#8250,#8251);
#6940=AXIS2_PLACEMENT_3D('',#11538,#8252,#8253);
#6941=AXIS2_PLACEMENT_3D('',#11539,#8254,#8255);
#6942=AXIS2_PLACEMENT_3D('',#11540,#8256,#8257);
#6943=AXIS2_PLACEMENT_3D('',#11542,#8258,#8259);
#6944=AXIS2_PLACEMENT_3D('',#11544,#8261,#8262);
#6945=AXIS2_PLACEMENT_3D('',#11546,#8263,#8264);
#6946=AXIS2_PLACEMENT_3D('',#11548,#8265,#8266);
#6947=AXIS2_PLACEMENT_3D('',#11549,#8267,#8268);
#6948=AXIS2_PLACEMENT_3D('',#11551,#8269,#8270);
#6949=AXIS2_PLACEMENT_3D('',#11553,#8272,#8273);
#6950=AXIS2_PLACEMENT_3D('',#11555,#8274,#8275);
#6951=AXIS2_PLACEMENT_3D('',#11557,#8277,#8278);
#6952=AXIS2_PLACEMENT_3D('',#11559,#8279,#8280);
#6953=AXIS2_PLACEMENT_3D('',#11561,#8282,#8283);
#6954=AXIS2_PLACEMENT_3D('',#11562,#8284,#8285);
#6955=AXIS2_PLACEMENT_3D('',#11564,#8287,#8288);
#6956=AXIS2_PLACEMENT_3D('',#11565,#8289,#8290);
#6957=AXIS2_PLACEMENT_3D('',#11568,#8291,#8292);
#6958=AXIS2_PLACEMENT_3D('',#11569,#8293,#8294);
#6959=AXIS2_PLACEMENT_3D('',#11572,#8295,#8296);
#6960=AXIS2_PLACEMENT_3D('',#11573,#8297,#8298);
#6961=AXIS2_PLACEMENT_3D('',#11576,#8299,#8300);
#6962=AXIS2_PLACEMENT_3D('',#11577,#8301,#8302);
#6963=AXIS2_PLACEMENT_3D('',#11580,#8303,#8304);
#6964=AXIS2_PLACEMENT_3D('',#11581,#8305,#8306);
#6965=AXIS2_PLACEMENT_3D('',#11584,#8307,#8308);
#6966=AXIS2_PLACEMENT_3D('',#11585,#8309,#8310);
#6967=AXIS2_PLACEMENT_3D('',#11588,#8311,#8312);
#6968=AXIS2_PLACEMENT_3D('',#11589,#8313,#8314);
#6969=AXIS2_PLACEMENT_3D('',#11592,#8315,#8316);
#6970=AXIS2_PLACEMENT_3D('',#11593,#8317,#8318);
#6971=AXIS2_PLACEMENT_3D('',#11594,#8319,#8320);
#6972=AXIS2_PLACEMENT_3D('',#11620,#8321,#8322);
#6973=AXIS2_PLACEMENT_3D('',#11644,#8323,#8324);
#6974=AXIS2_PLACEMENT_3D('',#11645,#8325,#8326);
#6975=AXIS2_PLACEMENT_3D('',#11647,#8327,#8328);
#6976=AXIS2_PLACEMENT_3D('',#11672,#8329,#8330);
#6977=AXIS2_PLACEMENT_3D('',#11697,#8331,#8332);
#6978=AXIS2_PLACEMENT_3D('',#11700,#8334,#8335);
#6979=AXIS2_PLACEMENT_3D('',#11702,#8336,#8337);
#6980=AXIS2_PLACEMENT_3D('',#11727,#8338,#8339);
#6981=AXIS2_PLACEMENT_3D('',#11752,#8340,#8341);
#6982=AXIS2_PLACEMENT_3D('',#11777,#8342,#8343);
#6983=AXIS2_PLACEMENT_3D('',#11801,#8344,#8345);
#6984=AXIS2_PLACEMENT_3D('',#11802,#8346,#8347);
#6985=AXIS2_PLACEMENT_3D('',#11804,#8348,#8349);
#6986=AXIS2_PLACEMENT_3D('',#11805,#8350,#8351);
#6987=AXIS2_PLACEMENT_3D('',#11806,#8352,#8353);
#6988=AXIS2_PLACEMENT_3D('',#11830,#8354,#8355);
#6989=AXIS2_PLACEMENT_3D('',#11831,#8356,#8357);
#6990=AXIS2_PLACEMENT_3D('',#11833,#8358,#8359);
#6991=AXIS2_PLACEMENT_3D('',#11834,#8360,#8361);
#6992=AXIS2_PLACEMENT_3D('',#11835,#8362,#8363);
#6993=AXIS2_PLACEMENT_3D('',#11859,#8364,#8365);
#6994=AXIS2_PLACEMENT_3D('',#11860,#8366,#8367);
#6995=AXIS2_PLACEMENT_3D('',#11862,#8368,#8369);
#6996=AXIS2_PLACEMENT_3D('',#11864,#8370,#8371);
#6997=AXIS2_PLACEMENT_3D('',#11865,#8372,#8373);
#6998=AXIS2_PLACEMENT_3D('',#11866,#8374,#8375);
#6999=AXIS2_PLACEMENT_3D('',#11890,#8376,#8377);
#7000=AXIS2_PLACEMENT_3D('',#11891,#8378,#8379);
#7001=AXIS2_PLACEMENT_3D('',#11893,#8380,#8381);
#7002=AXIS2_PLACEMENT_3D('',#11894,#8382,#8383);
#7003=AXIS2_PLACEMENT_3D('',#11895,#8384,#8385);
#7004=AXIS2_PLACEMENT_3D('',#11919,#8386,#8387);
#7005=AXIS2_PLACEMENT_3D('',#11920,#8388,#8389);
#7006=AXIS2_PLACEMENT_3D('',#11922,#8390,#8391);
#7007=AXIS2_PLACEMENT_3D('',#11923,#8392,#8393);
#7008=AXIS2_PLACEMENT_3D('',#11924,#8394,#8395);
#7009=AXIS2_PLACEMENT_3D('',#11948,#8396,#8397);
#7010=AXIS2_PLACEMENT_3D('',#11949,#8398,#8399);
#7011=AXIS2_PLACEMENT_3D('',#11951,#8400,#8401);
#7012=AXIS2_PLACEMENT_3D('',#11954,#8403,#8404);
#7013=AXIS2_PLACEMENT_3D('',#11978,#8405,#8406);
#7014=AXIS2_PLACEMENT_3D('',#11979,#8407,#8408);
#7015=AXIS2_PLACEMENT_3D('',#11980,#8409,#8410);
#7016=AXIS2_PLACEMENT_3D('',#11981,#8411,#8412);
#7017=AXIS2_PLACEMENT_3D('',#11982,#8413,#8414);
#7018=AXIS2_PLACEMENT_3D('',#11983,#8415,#8416);
#7019=AXIS2_PLACEMENT_3D('',#11984,#8417,#8418);
#7020=AXIS2_PLACEMENT_3D('',#11985,#8419,#8420);
#7021=AXIS2_PLACEMENT_3D('',#11986,#8421,#8422);
#7022=AXIS2_PLACEMENT_3D('',#11988,#8423,#8424);
#7023=AXIS2_PLACEMENT_3D('',#11990,#8425,#8426);
#7024=AXIS2_PLACEMENT_3D('',#11991,#8427,#8428);
#7025=AXIS2_PLACEMENT_3D('',#11993,#8429,#8430);
#7026=AXIS2_PLACEMENT_3D('',#11995,#8432,#8433);
#7027=AXIS2_PLACEMENT_3D('',#11997,#8434,#8435);
#7028=AXIS2_PLACEMENT_3D('',#11998,#8436,#8437);
#7029=AXIS2_PLACEMENT_3D('',#12000,#8439,#8440);
#7030=AXIS2_PLACEMENT_3D('',#12002,#8441,#8442);
#7031=AXIS2_PLACEMENT_3D('',#12004,#8443,#8444);
#7032=AXIS2_PLACEMENT_3D('',#12005,#8445,#8446);
#7033=AXIS2_PLACEMENT_3D('',#12007,#8447,#8448);
#7034=AXIS2_PLACEMENT_3D('',#12009,#8450,#8451);
#7035=AXIS2_PLACEMENT_3D('',#12011,#8452,#8453);
#7036=AXIS2_PLACEMENT_3D('',#12012,#8454,#8455);
#7037=AXIS2_PLACEMENT_3D('',#12014,#8457,#8458);
#7038=AXIS2_PLACEMENT_3D('',#12015,#8459,#8460);
#7039=AXIS2_PLACEMENT_3D('',#12016,#8461,#8462);
#7040=AXIS2_PLACEMENT_3D('',#12017,#8463,#8464);
#7041=AXIS2_PLACEMENT_3D('',#12018,#8465,#8466);
#7042=AXIS2_PLACEMENT_3D('',#12019,#8467,#8468);
#7043=AXIS2_PLACEMENT_3D('',#12020,#8469,#8470);
#7044=AXIS2_PLACEMENT_3D('',#12022,#8471,#8472);
#7045=AXIS2_PLACEMENT_3D('',#12023,#8473,#8474);
#7046=AXIS2_PLACEMENT_3D('',#12025,#8475,#8476);
#7047=AXIS2_PLACEMENT_3D('',#12027,#8478,#8479);
#7048=AXIS2_PLACEMENT_3D('',#12029,#8480,#8481);
#7049=AXIS2_PLACEMENT_3D('',#12031,#8483,#8484);
#7050=AXIS2_PLACEMENT_3D('',#12033,#8485,#8486);
#7051=AXIS2_PLACEMENT_3D('',#12035,#8488,#8489);
#7052=AXIS2_PLACEMENT_3D('',#12037,#8490,#8491);
#7053=AXIS2_PLACEMENT_3D('',#12038,#8492,#8493);
#7054=AXIS2_PLACEMENT_3D('',#12040,#8494,#8495);
#7055=AXIS2_PLACEMENT_3D('',#12042,#8497,#8498);
#7056=AXIS2_PLACEMENT_3D('',#12044,#8499,#8500);
#7057=AXIS2_PLACEMENT_3D('',#12046,#8502,#8503);
#7058=AXIS2_PLACEMENT_3D('',#12048,#8504,#8505);
#7059=AXIS2_PLACEMENT_3D('',#12050,#8507,#8508);
#7060=AXIS2_PLACEMENT_3D('',#12051,#8509,#8510);
#7061=AXIS2_PLACEMENT_3D('',#12060,#8515,#8516);
#7062=AXIS2_PLACEMENT_3D('',#12066,#8520,#8521);
#7063=AXIS2_PLACEMENT_3D('',#12072,#8525,#8526);
#7064=AXIS2_PLACEMENT_3D('',#12078,#8530,#8531);
#7065=AXIS2_PLACEMENT_3D('',#12084,#8535,#8536);
#7066=AXIS2_PLACEMENT_3D('',#12087,#8539,#8540);
#7067=AXIS2_PLACEMENT_3D('',#12088,#8541,#8542);
#7068=AXIS2_PLACEMENT_3D('',#12089,#8543,#8544);
#7069=AXIS2_PLACEMENT_3D('',#12090,#8545,#8546);
#7070=AXIS2_PLACEMENT_3D('',#12091,#8547,#8548);
#7071=AXIS2_PLACEMENT_3D('',#12094,#8549,#8550);
#7072=AXIS2_PLACEMENT_3D('',#12100,#8554,#8555);
#7073=AXIS2_PLACEMENT_3D('',#12106,#8559,#8560);
#7074=AXIS2_PLACEMENT_3D('',#12108,#8561,#8562);
#7075=AXIS2_PLACEMENT_3D('',#12112,#8565,#8566);
#7076=AXIS2_PLACEMENT_3D('',#12115,#8569,#8570);
#7077=AXIS2_PLACEMENT_3D('',#12116,#8571,#8572);
#7078=AXIS2_PLACEMENT_3D('',#12118,#8573,#8574);
#7079=AXIS2_PLACEMENT_3D('',#12120,#8575,#8576);
#7080=AXIS2_PLACEMENT_3D('',#12121,#8577,#8578);
#7081=AXIS2_PLACEMENT_3D('',#12123,#8579,#8580);
#7082=AXIS2_PLACEMENT_3D('',#12125,#8582,#8583);
#7083=AXIS2_PLACEMENT_3D('',#12127,#8584,#8585);
#7084=AXIS2_PLACEMENT_3D('',#12128,#8586,#8587);
#7085=AXIS2_PLACEMENT_3D('',#12130,#8588,#8589);
#7086=AXIS2_PLACEMENT_3D('',#12132,#8591,#8592);
#7087=AXIS2_PLACEMENT_3D('',#12134,#8593,#8594);
#7088=AXIS2_PLACEMENT_3D('',#12135,#8595,#8596);
#7089=AXIS2_PLACEMENT_3D('',#12137,#8597,#8598);
#7090=AXIS2_PLACEMENT_3D('',#12139,#8600,#8601);
#7091=AXIS2_PLACEMENT_3D('',#12141,#8602,#8603);
#7092=AXIS2_PLACEMENT_3D('',#12142,#8604,#8605);
#7093=AXIS2_PLACEMENT_3D('',#12144,#8606,#8607);
#7094=AXIS2_PLACEMENT_3D('',#12146,#8609,#8610);
#7095=AXIS2_PLACEMENT_3D('',#12148,#8611,#8612);
#7096=AXIS2_PLACEMENT_3D('',#12149,#8613,#8614);
#7097=AXIS2_PLACEMENT_3D('',#12151,#8615,#8616);
#7098=AXIS2_PLACEMENT_3D('',#12153,#8618,#8619);
#7099=AXIS2_PLACEMENT_3D('',#12155,#8620,#8621);
#7100=AXIS2_PLACEMENT_3D('',#12156,#8622,#8623);
#7101=AXIS2_PLACEMENT_3D('',#12158,#8625,#8626);
#7102=AXIS2_PLACEMENT_3D('',#12159,#8627,#8628);
#7103=AXIS2_PLACEMENT_3D('',#12162,#8629,#8630);
#7104=AXIS2_PLACEMENT_3D('',#12166,#8632,#8633);
#7105=AXIS2_PLACEMENT_3D('',#12168,#8635,#8636);
#7106=AXIS2_PLACEMENT_3D('',#12174,#8640,#8641);
#7107=AXIS2_PLACEMENT_3D('',#12176,#8642,#8643);
#7108=AXIS2_PLACEMENT_3D('',#12178,#8644,#8645);
#7109=AXIS2_PLACEMENT_3D('',#12180,#8647,#8648);
#7110=AXIS2_PLACEMENT_3D('',#12183,#8651,#8652);
#7111=AXIS2_PLACEMENT_3D('',#12185,#8653,#8654);
#7112=AXIS2_PLACEMENT_3D('',#12187,#8655,#8656);
#7113=AXIS2_PLACEMENT_3D('',#12188,#8657,#8658);
#7114=AXIS2_PLACEMENT_3D('',#12190,#8659,#8660);
#7115=AXIS2_PLACEMENT_3D('',#12192,#8662,#8663);
#7116=AXIS2_PLACEMENT_3D('',#12194,#8664,#8665);
#7117=AXIS2_PLACEMENT_3D('',#12195,#8666,#8667);
#7118=AXIS2_PLACEMENT_3D('',#12197,#8669,#8670);
#7119=AXIS2_PLACEMENT_3D('',#12198,#8671,#8672);
#7120=AXIS2_PLACEMENT_3D('',#12199,#8673,#8674);
#7121=AXIS2_PLACEMENT_3D('',#12200,#8675,#8676);
#7122=AXIS2_PLACEMENT_3D('',#12209,#8681,#8682);
#7123=AXIS2_PLACEMENT_3D('',#12215,#8686,#8687);
#7124=AXIS2_PLACEMENT_3D('',#12221,#8691,#8692);
#7125=AXIS2_PLACEMENT_3D('',#12227,#8696,#8697);
#7126=AXIS2_PLACEMENT_3D('',#12233,#8701,#8702);
#7127=AXIS2_PLACEMENT_3D('',#12236,#8705,#8706);
#7128=AXIS2_PLACEMENT_3D('',#12237,#8707,#8708);
#7129=AXIS2_PLACEMENT_3D('',#12238,#8709,#8710);
#7130=AXIS2_PLACEMENT_3D('',#12240,#8711,#8712);
#7131=AXIS2_PLACEMENT_3D('',#12241,#8713,#8714);
#7132=AXIS2_PLACEMENT_3D('',#12243,#8715,#8716);
#7133=AXIS2_PLACEMENT_3D('',#12244,#8717,#8718);
#7134=AXIS2_PLACEMENT_3D('',#12246,#8719,#8720);
#7135=AXIS2_PLACEMENT_3D('',#12248,#8722,#8723);
#7136=AXIS2_PLACEMENT_3D('',#12250,#8724,#8725);
#7137=AXIS2_PLACEMENT_3D('',#12252,#8727,#8728);
#7138=AXIS2_PLACEMENT_3D('',#12254,#8729,#8730);
#7139=AXIS2_PLACEMENT_3D('',#12256,#8732,#8733);
#7140=AXIS2_PLACEMENT_3D('',#12258,#8734,#8735);
#7141=AXIS2_PLACEMENT_3D('',#12259,#8736,#8737);
#7142=AXIS2_PLACEMENT_3D('',#12261,#8738,#8739);
#7143=AXIS2_PLACEMENT_3D('',#12263,#8741,#8742);
#7144=AXIS2_PLACEMENT_3D('',#12265,#8744,#8745);
#7145=AXIS2_PLACEMENT_3D('',#12266,#8746,#8747);
#7146=AXIS2_PLACEMENT_3D('',#12267,#8748,#8749);
#7147=AXIS2_PLACEMENT_3D('',#12269,#8750,#8751);
#7148=AXIS2_PLACEMENT_3D('',#12272,#8753,#8754);
#7149=AXIS2_PLACEMENT_3D('',#12273,#8755,#8756);
#7150=AXIS2_PLACEMENT_3D('',#12274,#8757,#8758);
#7151=AXIS2_PLACEMENT_3D('',#12276,#8759,#8760);
#7152=AXIS2_PLACEMENT_3D('',#12279,#8762,#8763);
#7153=AXIS2_PLACEMENT_3D('',#12280,#8764,#8765);
#7154=AXIS2_PLACEMENT_3D('',#12281,#8766,#8767);
#7155=AXIS2_PLACEMENT_3D('',#12290,#8772,#8773);
#7156=AXIS2_PLACEMENT_3D('',#12292,#8774,#8775);
#7157=AXIS2_PLACEMENT_3D('',#12296,#8778,#8779);
#7158=AXIS2_PLACEMENT_3D('',#12302,#8783,#8784);
#7159=AXIS2_PLACEMENT_3D('',#12304,#8786,#8787);
#7160=AXIS2_PLACEMENT_3D('',#12305,#8788,#8789);
#7161=AXIS2_PLACEMENT_3D('',#12306,#8790,#8791);
#7162=AXIS2_PLACEMENT_3D('',#12315,#8796,#8797);
#7163=AXIS2_PLACEMENT_3D('',#12317,#8798,#8799);
#7164=AXIS2_PLACEMENT_3D('',#12321,#8802,#8803);
#7165=AXIS2_PLACEMENT_3D('',#12327,#8807,#8808);
#7166=AXIS2_PLACEMENT_3D('',#12329,#8810,#8811);
#7167=AXIS2_PLACEMENT_3D('',#12330,#8812,#8813);
#7168=AXIS2_PLACEMENT_3D('',#12331,#8814,#8815);
#7169=AXIS2_PLACEMENT_3D('',#12333,#8816,#8817);
#7170=AXIS2_PLACEMENT_3D('',#12336,#8819,#8820);
#7171=AXIS2_PLACEMENT_3D('',#12337,#8821,#8822);
#7172=AXIS2_PLACEMENT_3D('',#12338,#8823,#8824);
#7173=AXIS2_PLACEMENT_3D('',#12339,#8825,#8826);
#7174=AXIS2_PLACEMENT_3D('',#12340,#8827,#8828);
#7175=AXIS2_PLACEMENT_3D('',#12342,#8829,#8830);
#7176=AXIS2_PLACEMENT_3D('',#12345,#8832,#8833);
#7177=AXIS2_PLACEMENT_3D('',#12346,#8834,#8835);
#7178=AXIS2_PLACEMENT_3D('',#12348,#8836,#8837);
#7179=AXIS2_PLACEMENT_3D('',#12351,#8839,#8840);
#7180=AXIS2_PLACEMENT_3D('',#12352,#8841,#8842);
#7181=AXIS2_PLACEMENT_3D('',#12353,#8843,#8844);
#7182=AXIS2_PLACEMENT_3D('',#12354,#8845,#8846);
#7183=AXIS2_PLACEMENT_3D('',#12355,#8847,#8848);
#7184=AXIS2_PLACEMENT_3D('',#12357,#8849,#8850);
#7185=AXIS2_PLACEMENT_3D('',#12360,#8852,#8853);
#7186=AXIS2_PLACEMENT_3D('',#12361,#8854,#8855);
#7187=AXIS2_PLACEMENT_3D('',#12363,#8856,#8857);
#7188=AXIS2_PLACEMENT_3D('',#12366,#8859,#8860);
#7189=AXIS2_PLACEMENT_3D('',#12367,#8861,#8862);
#7190=AXIS2_PLACEMENT_3D('',#12368,#8863,#8864);
#7191=AXIS2_PLACEMENT_3D('',#12369,#8865,#8866);
#7192=AXIS2_PLACEMENT_3D('',#12370,#8867,#8868);
#7193=AXIS2_PLACEMENT_3D('',#12372,#8869,#8870);
#7194=AXIS2_PLACEMENT_3D('',#12375,#8872,#8873);
#7195=AXIS2_PLACEMENT_3D('',#12376,#8874,#8875);
#7196=AXIS2_PLACEMENT_3D('',#12378,#8876,#8877);
#7197=AXIS2_PLACEMENT_3D('',#12381,#8879,#8880);
#7198=AXIS2_PLACEMENT_3D('',#12382,#8881,#8882);
#7199=AXIS2_PLACEMENT_3D('',#12383,#8883,#8884);
#7200=AXIS2_PLACEMENT_3D('',#12384,#8885,#8886);
#7201=AXIS2_PLACEMENT_3D('',#12385,#8887,#8888);
#7202=AXIS2_PLACEMENT_3D('',#12387,#8889,#8890);
#7203=AXIS2_PLACEMENT_3D('',#12390,#8892,#8893);
#7204=AXIS2_PLACEMENT_3D('',#12391,#8894,#8895);
#7205=AXIS2_PLACEMENT_3D('',#12393,#8896,#8897);
#7206=AXIS2_PLACEMENT_3D('',#12396,#8899,#8900);
#7207=AXIS2_PLACEMENT_3D('',#12397,#8901,#8902);
#7208=AXIS2_PLACEMENT_3D('',#12398,#8903,#8904);
#7209=AXIS2_PLACEMENT_3D('',#12399,#8905,#8906);
#7210=AXIS2_PLACEMENT_3D('',#12400,#8907,#8908);
#7211=AXIS2_PLACEMENT_3D('',#12409,#8913,#8914);
#7212=AXIS2_PLACEMENT_3D('',#12415,#8918,#8919);
#7213=AXIS2_PLACEMENT_3D('',#12421,#8923,#8924);
#7214=AXIS2_PLACEMENT_3D('',#12423,#8925,#8926);
#7215=AXIS2_PLACEMENT_3D('',#12424,#8927,#8928);
#7216=AXIS2_PLACEMENT_3D('',#12425,#8929,#8930);
#7217=AXIS2_PLACEMENT_3D('',#12426,#8931,#8932);
#7218=AXIS2_PLACEMENT_3D('',#12427,#8933,#8934);
#7219=AXIS2_PLACEMENT_3D('',#12429,#8935,#8936);
#7220=AXIS2_PLACEMENT_3D('',#12432,#8938,#8939);
#7221=AXIS2_PLACEMENT_3D('',#12433,#8940,#8941);
#7222=AXIS2_PLACEMENT_3D('',#12436,#8943,#8944);
#7223=AXIS2_PLACEMENT_3D('',#12437,#8945,#8946);
#7224=AXIS2_PLACEMENT_3D('',#12438,#8947,#8948);
#7225=AXIS2_PLACEMENT_3D('',#12440,#8949,#8950);
#7226=AXIS2_PLACEMENT_3D('',#12443,#8952,#8953);
#7227=AXIS2_PLACEMENT_3D('',#12444,#8954,#8955);
#7228=AXIS2_PLACEMENT_3D('',#12445,#8956,#8957);
#7229=AXIS2_PLACEMENT_3D('',#12446,#8958,#8959);
#7230=AXIS2_PLACEMENT_3D('',#12447,#8960,#8961);
#7231=AXIS2_PLACEMENT_3D('',#12449,#8962,#8963);
#7232=AXIS2_PLACEMENT_3D('',#12452,#8965,#8966);
#7233=AXIS2_PLACEMENT_3D('',#12453,#8967,#8968);
#7234=AXIS2_PLACEMENT_3D('',#12462,#8973,#8974);
#7235=AXIS2_PLACEMENT_3D('',#12468,#8978,#8979);
#7236=AXIS2_PLACEMENT_3D('',#12474,#8983,#8984);
#7237=AXIS2_PLACEMENT_3D('',#12476,#8985,#8986);
#7238=AXIS2_PLACEMENT_3D('',#12477,#8987,#8988);
#7239=AXIS2_PLACEMENT_3D('',#12478,#8989,#8990);
#7240=AXIS2_PLACEMENT_3D('',#12479,#8991,#8992);
#7241=AXIS2_PLACEMENT_3D('',#12480,#8993,#8994);
#7242=AXIS2_PLACEMENT_3D('',#12485,#8996,#8997);
#7243=AXIS2_PLACEMENT_3D('',#12488,#8999,#9000);
#7244=AXIS2_PLACEMENT_3D('',#12489,#9001,#9002);
#7245=AXIS2_PLACEMENT_3D('',#12493,#9004,#9005);
#7246=AXIS2_PLACEMENT_3D('',#12495,#9007,#9008);
#7247=AXIS2_PLACEMENT_3D('',#12499,#9011,#9012);
#7248=AXIS2_PLACEMENT_3D('',#12503,#9015,#9016);
#7249=AXIS2_PLACEMENT_3D('',#12504,#9017,#9018);
#7250=AXIS2_PLACEMENT_3D('',#12505,#9019,#9020);
#7251=AXIS2_PLACEMENT_3D('',#12508,#9022,#9023);
#7252=AXIS2_PLACEMENT_3D('',#12509,#9024,#9025);
#7253=AXIS2_PLACEMENT_3D('',#12510,#9026,#9027);
#7254=AXIS2_PLACEMENT_3D('',#12511,#9028,#9029);
#7255=AXIS2_PLACEMENT_3D('',#12513,#9030,#9031);
#7256=AXIS2_PLACEMENT_3D('',#12516,#9033,#9034);
#7257=AXIS2_PLACEMENT_3D('',#12517,#9035,#9036);
#7258=AXIS2_PLACEMENT_3D('',#12518,#9037,#9038);
#7259=AXIS2_PLACEMENT_3D('',#12520,#9039,#9040);
#7260=AXIS2_PLACEMENT_3D('',#12523,#9042,#9043);
#7261=AXIS2_PLACEMENT_3D('',#12524,#9044,#9045);
#7262=AXIS2_PLACEMENT_3D('',#12525,#9046,#9047);
#7263=AXIS2_PLACEMENT_3D('',#12526,#9048,#9049);
#7264=AXIS2_PLACEMENT_3D('',#12527,#9050,#9051);
#7265=AXIS2_PLACEMENT_3D('',#12529,#9052,#9053);
#7266=AXIS2_PLACEMENT_3D('',#12532,#9055,#9056);
#7267=AXIS2_PLACEMENT_3D('',#12533,#9057,#9058);
#7268=AXIS2_PLACEMENT_3D('',#12535,#9059,#9060);
#7269=AXIS2_PLACEMENT_3D('',#12538,#9062,#9063);
#7270=AXIS2_PLACEMENT_3D('',#12539,#9064,#9065);
#7271=AXIS2_PLACEMENT_3D('',#12540,#9066,#9067);
#7272=AXIS2_PLACEMENT_3D('',#12541,#9068,#9069);
#7273=AXIS2_PLACEMENT_3D('',#12542,#9070,#9071);
#7274=AXIS2_PLACEMENT_3D('',#12544,#9072,#9073);
#7275=AXIS2_PLACEMENT_3D('',#12547,#9075,#9076);
#7276=AXIS2_PLACEMENT_3D('',#12548,#9077,#9078);
#7277=AXIS2_PLACEMENT_3D('',#12550,#9079,#9080);
#7278=AXIS2_PLACEMENT_3D('',#12553,#9082,#9083);
#7279=AXIS2_PLACEMENT_3D('',#12554,#9084,#9085);
#7280=AXIS2_PLACEMENT_3D('',#12555,#9086,#9087);
#7281=AXIS2_PLACEMENT_3D('',#12556,#9088,#9089);
#7282=AXIS2_PLACEMENT_3D('',#12557,#9090,#9091);
#7283=AXIS2_PLACEMENT_3D('',#12574,#9100,#9101);
#7284=AXIS2_PLACEMENT_3D('',#12580,#9105,#9106);
#7285=AXIS2_PLACEMENT_3D('',#12584,#9109,#9110);
#7286=AXIS2_PLACEMENT_3D('',#12588,#9113,#9114);
#7287=AXIS2_PLACEMENT_3D('',#12592,#9117,#9118);
#7288=AXIS2_PLACEMENT_3D('',#12600,#9123,#9124);
#7289=AXIS2_PLACEMENT_3D('',#12602,#9126,#9127);
#7290=AXIS2_PLACEMENT_3D('',#12604,#9129,#9130);
#7291=AXIS2_PLACEMENT_3D('',#12606,#9132,#9133);
#7292=AXIS2_PLACEMENT_3D('',#12607,#9134,#9135);
#7293=AXIS2_PLACEMENT_3D('',#12608,#9136,#9137);
#7294=AXIS2_PLACEMENT_3D('',#12610,#9138,#9139);
#7295=AXIS2_PLACEMENT_3D('',#12611,#9140,#9141);
#7296=AXIS2_PLACEMENT_3D('',#12613,#9142,#9143);
#7297=AXIS2_PLACEMENT_3D('',#12615,#9145,#9146);
#7298=AXIS2_PLACEMENT_3D('',#12617,#9147,#9148);
#7299=AXIS2_PLACEMENT_3D('',#12619,#9150,#9151);
#7300=AXIS2_PLACEMENT_3D('',#12621,#9152,#9153);
#7301=AXIS2_PLACEMENT_3D('',#12623,#9155,#9156);
#7302=AXIS2_PLACEMENT_3D('',#12625,#9157,#9158);
#7303=AXIS2_PLACEMENT_3D('',#12626,#9159,#9160);
#7304=AXIS2_PLACEMENT_3D('',#12628,#9161,#9162);
#7305=AXIS2_PLACEMENT_3D('',#12630,#9164,#9165);
#7306=AXIS2_PLACEMENT_3D('',#12632,#9166,#9167);
#7307=AXIS2_PLACEMENT_3D('',#12634,#9169,#9170);
#7308=AXIS2_PLACEMENT_3D('',#12636,#9171,#9172);
#7309=AXIS2_PLACEMENT_3D('',#12638,#9174,#9175);
#7310=AXIS2_PLACEMENT_3D('',#12639,#9176,#9177);
#7311=AXIS2_PLACEMENT_3D('',#12648,#9182,#9183);
#7312=AXIS2_PLACEMENT_3D('',#12654,#9187,#9188);
#7313=AXIS2_PLACEMENT_3D('',#12660,#9192,#9193);
#7314=AXIS2_PLACEMENT_3D('',#12666,#9197,#9198);
#7315=AXIS2_PLACEMENT_3D('',#12672,#9202,#9203);
#7316=AXIS2_PLACEMENT_3D('',#12675,#9206,#9207);
#7317=AXIS2_PLACEMENT_3D('',#12676,#9208,#9209);
#7318=AXIS2_PLACEMENT_3D('',#12677,#9210,#9211);
#7319=AXIS2_PLACEMENT_3D('',#12678,#9212,#9213);
#7320=AXIS2_PLACEMENT_3D('',#12679,#9214,#9215);
#7321=AXIS2_PLACEMENT_3D('',#12680,#9216,#9217);
#7322=AXIS2_PLACEMENT_3D('',#12681,#9218,#9219);
#7323=AXIS2_PLACEMENT_3D('',#12682,#9220,#9221);
#7324=AXIS2_PLACEMENT_3D('',#12683,#9222,#9223);
#7325=AXIS2_PLACEMENT_3D('',#12684,#9224,#9225);
#7326=AXIS2_PLACEMENT_3D('',#12685,#9226,#9227);
#7327=AXIS2_PLACEMENT_3D('',#12686,#9228,#9229);
#7328=AXIS2_PLACEMENT_3D('',#12687,#9230,#9231);
#7329=AXIS2_PLACEMENT_3D('',#12688,#9232,#9233);
#7330=AXIS2_PLACEMENT_3D('',#12689,#9234,#9235);
#7331=AXIS2_PLACEMENT_3D('',#12690,#9236,#9237);
#7332=AXIS2_PLACEMENT_3D('',#12691,#9238,#9239);
#7333=AXIS2_PLACEMENT_3D('',#12692,#9240,#9241);
#7334=AXIS2_PLACEMENT_3D('',#12693,#9242,#9243);
#7335=AXIS2_PLACEMENT_3D('',#12694,#9244,#9245);
#7336=AXIS2_PLACEMENT_3D('',#12695,#9246,#9247);
#7337=AXIS2_PLACEMENT_3D('',#12696,#9248,#9249);
#7338=AXIS2_PLACEMENT_3D('',#12697,#9250,#9251);
#7339=AXIS2_PLACEMENT_3D('',#12698,#9252,#9253);
#7340=AXIS2_PLACEMENT_3D('',#12699,#9254,#9255);
#7341=AXIS2_PLACEMENT_3D('',#12700,#9256,#9257);
#7342=AXIS2_PLACEMENT_3D('',#12701,#9258,#9259);
#7343=AXIS2_PLACEMENT_3D('',#12702,#9260,#9261);
#7344=AXIS2_PLACEMENT_3D('',#12703,#9262,#9263);
#7345=AXIS2_PLACEMENT_3D('',#12704,#9264,#9265);
#7346=AXIS2_PLACEMENT_3D('',#12705,#9266,#9267);
#7347=AXIS2_PLACEMENT_3D('',#12706,#9268,#9269);
#7348=AXIS2_PLACEMENT_3D('',#12707,#9270,#9271);
#7349=AXIS2_PLACEMENT_3D('',#12708,#9272,#9273);
#7350=AXIS2_PLACEMENT_3D('',#12709,#9274,#9275);
#7351=AXIS2_PLACEMENT_3D('',#12710,#9276,#9277);
#7352=AXIS2_PLACEMENT_3D('',#12711,#9278,#9279);
#7353=AXIS2_PLACEMENT_3D('',#12712,#9280,#9281);
#7354=AXIS2_PLACEMENT_3D('',#12713,#9282,#9283);
#7355=AXIS2_PLACEMENT_3D('',#12714,#9284,#9285);
#7356=AXIS2_PLACEMENT_3D('',#12715,#9286,#9287);
#7357=AXIS2_PLACEMENT_3D('',#12716,#9288,#9289);
#7358=AXIS2_PLACEMENT_3D('',#12717,#9290,#9291);
#7359=AXIS2_PLACEMENT_3D('',#12718,#9292,#9293);
#7360=AXIS2_PLACEMENT_3D('',#12719,#9294,#9295);
#7361=AXIS2_PLACEMENT_3D('',#12720,#9296,#9297);
#7362=AXIS2_PLACEMENT_3D('',#12721,#9298,#9299);
#7363=AXIS2_PLACEMENT_3D('',#12722,#9300,#9301);
#7364=AXIS2_PLACEMENT_3D('',#12723,#9302,#9303);
#7365=AXIS2_PLACEMENT_3D('',#12724,#9304,#9305);
#7366=AXIS2_PLACEMENT_3D('',#12725,#9306,#9307);
#7367=AXIS2_PLACEMENT_3D('',#12726,#9308,#9309);
#7368=AXIS2_PLACEMENT_3D('',#12727,#9310,#9311);
#7369=AXIS2_PLACEMENT_3D('',#12728,#9312,#9313);
#7370=AXIS2_PLACEMENT_3D('',#12729,#9314,#9315);
#7371=AXIS2_PLACEMENT_3D('',#12730,#9316,#9317);
#7372=AXIS2_PLACEMENT_3D('',#12731,#9318,#9319);
#7373=AXIS2_PLACEMENT_3D('',#12732,#9320,#9321);
#7374=AXIS2_PLACEMENT_3D('',#12733,#9322,#9323);
#7375=AXIS2_PLACEMENT_3D('',#12734,#9324,#9325);
#7376=AXIS2_PLACEMENT_3D('',#12735,#9326,#9327);
#7377=AXIS2_PLACEMENT_3D('',#12737,#9328,#9329);
#7378=AXIS2_PLACEMENT_3D('',#12740,#9331,#9332);
#7379=AXIS2_PLACEMENT_3D('',#12741,#9333,#9334);
#7380=AXIS2_PLACEMENT_3D('',#12750,#9339,#9340);
#7381=AXIS2_PLACEMENT_3D('',#12756,#9344,#9345);
#7382=AXIS2_PLACEMENT_3D('',#12762,#9349,#9350);
#7383=AXIS2_PLACEMENT_3D('',#12765,#9353,#9354);
#7384=AXIS2_PLACEMENT_3D('',#12766,#9355,#9356);
#7385=AXIS2_PLACEMENT_3D('',#12767,#9357,#9358);
#7386=AXIS2_PLACEMENT_3D('',#12768,#9359,#9360);
#7387=AXIS2_PLACEMENT_3D('',#12770,#9361,#9362);
#7388=AXIS2_PLACEMENT_3D('',#12772,#9363,#9364);
#7389=AXIS2_PLACEMENT_3D('',#12773,#9365,#9366);
#7390=AXIS2_PLACEMENT_3D('',#12775,#9367,#9368);
#7391=AXIS2_PLACEMENT_3D('',#12777,#9370,#9371);
#7392=AXIS2_PLACEMENT_3D('',#12778,#9372,#9373);
#7393=AXIS2_PLACEMENT_3D('',#12780,#9374,#9375);
#7394=AXIS2_PLACEMENT_3D('',#12783,#9377,#9378);
#7395=AXIS2_PLACEMENT_3D('',#12784,#9379,#9380);
#7396=AXIS2_PLACEMENT_3D('',#12785,#9381,#9382);
#7397=AXIS2_PLACEMENT_3D('',#12788,#9384,#9385);
#7398=AXIS2_PLACEMENT_3D('',#12789,#9386,#9387);
#7399=AXIS2_PLACEMENT_3D('',#12790,#9388,#9389);
#7400=AXIS2_PLACEMENT_3D('',#12791,#9390,#9391);
#7401=AXIS2_PLACEMENT_3D('',#12793,#9392,#9393);
#7402=AXIS2_PLACEMENT_3D('',#12796,#9395,#9396);
#7403=AXIS2_PLACEMENT_3D('',#12797,#9397,#9398);
#7404=AXIS2_PLACEMENT_3D('',#12799,#9399,#9400);
#7405=AXIS2_PLACEMENT_3D('',#12802,#9402,#9403);
#7406=AXIS2_PLACEMENT_3D('',#12803,#9404,#9405);
#7407=AXIS2_PLACEMENT_3D('',#12804,#9406,#9407);
#7408=AXIS2_PLACEMENT_3D('',#12805,#9408,#9409);
#7409=AXIS2_PLACEMENT_3D('',#12806,#9410,#9411);
#7410=AXIS2_PLACEMENT_3D('',#12807,#9412,#9413);
#7411=AXIS2_PLACEMENT_3D('',#12808,#9414,#9415);
#7412=AXIS2_PLACEMENT_3D('',#12809,#9416,#9417);
#7413=AXIS2_PLACEMENT_3D('',#12810,#9418,#9419);
#7414=DIRECTION('axis',(0.,0.,1.));
#7415=DIRECTION('refdir',(1.,0.,0.));
#7416=DIRECTION('axis',(0.,0.,1.));
#7417=DIRECTION('refdir',(1.,0.,0.));
#7418=DIRECTION('axis',(0.,0.,1.));
#7419=DIRECTION('refdir',(1.,0.,0.));
#7420=DIRECTION('center_axis',(0.,-1.,0.));
#7421=DIRECTION('ref_axis',(1.,0.,0.));
#7422=DIRECTION('',(-1.,0.,0.));
#7423=DIRECTION('',(0.,0.,1.));
#7424=DIRECTION('',(1.,0.,0.));
#7425=DIRECTION('',(0.,0.,1.));
#7426=DIRECTION('center_axis',(-1.,0.,0.));
#7427=DIRECTION('ref_axis',(0.,-1.,0.));
#7428=DIRECTION('',(0.,1.,0.));
#7429=DIRECTION('',(0.,-1.,0.));
#7430=DIRECTION('',(0.,0.,1.));
#7431=DIRECTION('center_axis',(0.,1.,0.));
#7432=DIRECTION('ref_axis',(-1.,0.,0.));
#7433=DIRECTION('',(1.,0.,0.));
#7434=DIRECTION('',(-1.,0.,0.));
#7435=DIRECTION('',(0.,0.,1.));
#7436=DIRECTION('center_axis',(1.,0.,0.));
#7437=DIRECTION('ref_axis',(0.,1.,0.));
#7438=DIRECTION('',(0.,-1.,0.));
#7439=DIRECTION('',(0.,1.,0.));
#7440=DIRECTION('center_axis',(0.,0.,1.));
#7441=DIRECTION('ref_axis',(1.,0.,0.));
#7442=DIRECTION('center_axis',(0.,0.,1.));
#7443=DIRECTION('ref_axis',(1.,0.,0.));
#7444=DIRECTION('center_axis',(0.,0.,1.));
#7445=DIRECTION('ref_axis',(1.,0.,0.));
#7446=DIRECTION('',(0.,0.,1.));
#7447=DIRECTION('center_axis',(0.,0.,-1.));
#7448=DIRECTION('ref_axis',(1.,0.,0.));
#7449=DIRECTION('center_axis',(0.,0.,1.));
#7450=DIRECTION('ref_axis',(1.,0.,0.));
#7451=DIRECTION('center_axis',(0.,0.,1.));
#7452=DIRECTION('ref_axis',(1.,0.,0.));
#7453=DIRECTION('',(0.,0.,1.));
#7454=DIRECTION('center_axis',(0.,0.,-1.));
#7455=DIRECTION('ref_axis',(1.,0.,0.));
#7456=DIRECTION('center_axis',(0.,0.,1.));
#7457=DIRECTION('ref_axis',(1.,0.,0.));
#7458=DIRECTION('center_axis',(0.,0.,1.));
#7459=DIRECTION('ref_axis',(1.,0.,0.));
#7460=DIRECTION('',(0.,0.,1.));
#7461=DIRECTION('center_axis',(0.,0.,-1.));
#7462=DIRECTION('ref_axis',(1.,0.,0.));
#7463=DIRECTION('center_axis',(0.,0.,1.));
#7464=DIRECTION('ref_axis',(1.,0.,0.));
#7465=DIRECTION('center_axis',(0.,0.,1.));
#7466=DIRECTION('ref_axis',(1.,0.,0.));
#7467=DIRECTION('',(0.,0.,1.));
#7468=DIRECTION('center_axis',(0.,0.,-1.));
#7469=DIRECTION('ref_axis',(1.,0.,0.));
#7470=DIRECTION('center_axis',(0.,0.,1.));
#7471=DIRECTION('ref_axis',(1.,0.,0.));
#7472=DIRECTION('center_axis',(0.,0.,1.));
#7473=DIRECTION('ref_axis',(1.,0.,0.));
#7474=DIRECTION('',(0.,0.,1.));
#7475=DIRECTION('center_axis',(0.,0.,-1.));
#7476=DIRECTION('ref_axis',(1.,0.,0.));
#7477=DIRECTION('center_axis',(0.,0.,1.));
#7478=DIRECTION('ref_axis',(1.,0.,0.));
#7479=DIRECTION('center_axis',(0.,0.,1.));
#7480=DIRECTION('ref_axis',(1.,0.,0.));
#7481=DIRECTION('',(0.,0.,1.));
#7482=DIRECTION('center_axis',(0.,0.,-1.));
#7483=DIRECTION('ref_axis',(1.,0.,0.));
#7484=DIRECTION('center_axis',(0.,1.,0.));
#7485=DIRECTION('ref_axis',(-1.,0.,0.));
#7486=DIRECTION('',(-1.,0.,0.));
#7487=DIRECTION('',(0.,0.,1.));
#7488=DIRECTION('',(-1.,0.,0.));
#7489=DIRECTION('',(0.,0.,1.));
#7490=DIRECTION('center_axis',(1.,0.,0.));
#7491=DIRECTION('ref_axis',(0.,1.,0.));
#7492=DIRECTION('',(0.,1.,0.));
#7493=DIRECTION('',(0.,1.,0.));
#7494=DIRECTION('',(0.,0.,1.));
#7495=DIRECTION('center_axis',(0.,-1.,0.));
#7496=DIRECTION('ref_axis',(1.,0.,0.));
#7497=DIRECTION('',(1.,0.,0.));
#7498=DIRECTION('',(1.,0.,0.));
#7499=DIRECTION('',(0.,0.,1.));
#7500=DIRECTION('center_axis',(-1.,0.,0.));
#7501=DIRECTION('ref_axis',(0.,-1.,0.));
#7502=DIRECTION('',(0.,-1.,0.));
#7503=DIRECTION('',(0.,-1.,0.));
#7504=DIRECTION('center_axis',(0.,0.,1.));
#7505=DIRECTION('ref_axis',(1.,0.,0.));
#7506=DIRECTION('center_axis',(0.,0.,1.));
#7507=DIRECTION('ref_axis',(1.,0.,0.));
#7508=DIRECTION('axis',(0.,0.,1.));
#7509=DIRECTION('refdir',(1.,0.,0.));
#7510=DIRECTION('center_axis',(0.,1.,0.));
#7511=DIRECTION('ref_axis',(-1.,0.,0.));
#7512=DIRECTION('',(-1.,0.,0.));
#7513=DIRECTION('',(0.,0.,1.));
#7514=DIRECTION('',(-1.,0.,0.));
#7515=DIRECTION('',(0.,0.,1.));
#7516=DIRECTION('center_axis',(1.,0.,0.));
#7517=DIRECTION('ref_axis',(0.,1.,0.));
#7518=DIRECTION('',(0.,1.,0.));
#7519=DIRECTION('',(0.,1.,0.));
#7520=DIRECTION('',(0.,0.,1.));
#7521=DIRECTION('center_axis',(0.,-1.,0.));
#7522=DIRECTION('ref_axis',(1.,0.,0.));
#7523=DIRECTION('',(1.,0.,0.));
#7524=DIRECTION('',(1.,0.,0.));
#7525=DIRECTION('',(0.,0.,1.));
#7526=DIRECTION('center_axis',(-1.,0.,0.));
#7527=DIRECTION('ref_axis',(0.,-1.,0.));
#7528=DIRECTION('',(0.,-1.,0.));
#7529=DIRECTION('',(0.,-1.,0.));
#7530=DIRECTION('center_axis',(0.,0.,1.));
#7531=DIRECTION('ref_axis',(1.,0.,0.));
#7532=DIRECTION('center_axis',(0.,0.,1.));
#7533=DIRECTION('ref_axis',(1.,0.,0.));
#7534=DIRECTION('axis',(0.,0.,1.));
#7535=DIRECTION('refdir',(1.,0.,0.));
#7536=DIRECTION('center_axis',(0.,1.,0.));
#7537=DIRECTION('ref_axis',(-1.,0.,0.));
#7538=DIRECTION('',(-1.,0.,0.));
#7539=DIRECTION('',(0.,0.,1.));
#7540=DIRECTION('',(-1.,0.,0.));
#7541=DIRECTION('',(0.,0.,1.));
#7542=DIRECTION('center_axis',(1.,0.,0.));
#7543=DIRECTION('ref_axis',(0.,1.,0.));
#7544=DIRECTION('',(0.,1.,0.));
#7545=DIRECTION('',(0.,1.,0.));
#7546=DIRECTION('',(0.,0.,1.));
#7547=DIRECTION('center_axis',(0.,-1.,0.));
#7548=DIRECTION('ref_axis',(1.,0.,0.));
#7549=DIRECTION('',(1.,0.,0.));
#7550=DIRECTION('',(1.,0.,0.));
#7551=DIRECTION('',(0.,0.,1.));
#7552=DIRECTION('center_axis',(-1.,0.,0.));
#7553=DIRECTION('ref_axis',(0.,-1.,0.));
#7554=DIRECTION('',(0.,-1.,0.));
#7555=DIRECTION('',(0.,-1.,0.));
#7556=DIRECTION('center_axis',(0.,0.,1.));
#7557=DIRECTION('ref_axis',(1.,0.,0.));
#7558=DIRECTION('center_axis',(0.,0.,1.));
#7559=DIRECTION('ref_axis',(1.,0.,0.));
#7560=DIRECTION('axis',(0.,0.,1.));
#7561=DIRECTION('refdir',(1.,0.,0.));
#7562=DIRECTION('center_axis',(0.,0.,1.));
#7563=DIRECTION('ref_axis',(1.,0.,0.));
#7564=DIRECTION('center_axis',(0.,0.,1.));
#7565=DIRECTION('ref_axis',(1.,0.,0.));
#7566=DIRECTION('',(0.,0.,1.));
#7567=DIRECTION('center_axis',(0.,0.,-1.));
#7568=DIRECTION('ref_axis',(1.,0.,0.));
#7569=DIRECTION('center_axis',(0.,0.,1.));
#7570=DIRECTION('ref_axis',(1.,0.,0.));
#7571=DIRECTION('center_axis',(0.,0.,1.));
#7572=DIRECTION('ref_axis',(1.,0.,0.));
#7573=DIRECTION('',(0.,0.,1.));
#7574=DIRECTION('center_axis',(0.,0.,-1.));
#7575=DIRECTION('ref_axis',(1.,0.,0.));
#7576=DIRECTION('center_axis',(0.,1.,0.));
#7577=DIRECTION('ref_axis',(1.,0.,0.));
#7578=DIRECTION('center_axis',(0.,1.,0.));
#7579=DIRECTION('ref_axis',(1.,0.,0.));
#7580=DIRECTION('',(0.,1.,0.));
#7581=DIRECTION('center_axis',(0.,-1.,0.));
#7582=DIRECTION('ref_axis',(1.,0.,0.));
#7583=DIRECTION('center_axis',(0.,1.,0.));
#7584=DIRECTION('ref_axis',(1.,0.,0.));
#7585=DIRECTION('center_axis',(0.,1.,0.));
#7586=DIRECTION('ref_axis',(1.,0.,0.));
#7587=DIRECTION('',(0.,1.,0.));
#7588=DIRECTION('center_axis',(0.,-1.,0.));
#7589=DIRECTION('ref_axis',(1.,0.,0.));
#7590=DIRECTION('center_axis',(0.,1.,0.));
#7591=DIRECTION('ref_axis',(1.,0.,0.));
#7592=DIRECTION('center_axis',(0.,1.,0.));
#7593=DIRECTION('ref_axis',(1.,0.,0.));
#7594=DIRECTION('',(0.,1.,0.));
#7595=DIRECTION('center_axis',(0.,-1.,0.));
#7596=DIRECTION('ref_axis',(1.,0.,0.));
#7597=DIRECTION('center_axis',(0.,1.,0.));
#7598=DIRECTION('ref_axis',(1.,0.,0.));
#7599=DIRECTION('center_axis',(0.,1.,0.));
#7600=DIRECTION('ref_axis',(1.,0.,0.));
#7601=DIRECTION('',(0.,1.,0.));
#7602=DIRECTION('center_axis',(0.,-1.,0.));
#7603=DIRECTION('ref_axis',(1.,0.,0.));
#7604=DIRECTION('center_axis',(0.,1.,0.));
#7605=DIRECTION('ref_axis',(1.,0.,0.));
#7606=DIRECTION('center_axis',(0.,1.,0.));
#7607=DIRECTION('ref_axis',(1.,0.,0.));
#7608=DIRECTION('',(0.,1.,0.));
#7609=DIRECTION('center_axis',(0.,-1.,0.));
#7610=DIRECTION('ref_axis',(1.,0.,0.));
#7611=DIRECTION('center_axis',(0.,0.,1.));
#7612=DIRECTION('ref_axis',(1.,0.,0.));
#7613=DIRECTION('',(0.,1.,0.));
#7614=DIRECTION('',(-1.,0.,0.));
#7615=DIRECTION('',(0.,1.,0.));
#7616=DIRECTION('',(1.,0.,0.));
#7617=DIRECTION('center_axis',(0.,0.,1.));
#7618=DIRECTION('ref_axis',(1.,0.,0.));
#7619=DIRECTION('',(0.,-1.,0.));
#7620=DIRECTION('',(1.,0.,0.));
#7621=DIRECTION('',(0.,1.,0.));
#7622=DIRECTION('',(-1.,0.,0.));
#7623=DIRECTION('center_axis',(-1.,0.,0.));
#7624=DIRECTION('ref_axis',(0.,0.,1.));
#7625=DIRECTION('',(0.,0.,-1.));
#7626=DIRECTION('',(0.,0.,1.));
#7627=DIRECTION('',(0.,1.,0.));
#7628=DIRECTION('center_axis',(1.,0.,0.));
#7629=DIRECTION('ref_axis',(0.,0.,-1.));
#7630=DIRECTION('',(0.,0.,1.));
#7631=DIRECTION('',(0.,1.,0.));
#7632=DIRECTION('',(0.,0.,-1.));
#7633=DIRECTION('center_axis',(0.,-1.,0.));
#7634=DIRECTION('ref_axis',(1.,0.,0.));
#7635=DIRECTION('',(0.,0.,1.));
#7636=DIRECTION('',(1.,0.,0.));
#7637=DIRECTION('',(0.,0.,1.));
#7638=DIRECTION('',(1.,0.,0.));
#7639=DIRECTION('center_axis',(1.,0.,0.));
#7640=DIRECTION('ref_axis',(0.,1.,0.));
#7641=DIRECTION('',(0.,0.,1.));
#7642=DIRECTION('',(0.,1.,0.));
#7643=DIRECTION('center_axis',(0.,1.,0.));
#7644=DIRECTION('ref_axis',(-1.,0.,0.));
#7645=DIRECTION('',(0.,0.,1.));
#7646=DIRECTION('',(-1.,0.,0.));
#7647=DIRECTION('',(-1.,0.,0.));
#7648=DIRECTION('center_axis',(-1.,0.,0.));
#7649=DIRECTION('ref_axis',(0.,-1.,0.));
#7650=DIRECTION('',(0.,-1.,0.));
#7651=DIRECTION('center_axis',(0.,0.,1.));
#7652=DIRECTION('ref_axis',(1.,0.,0.));
#7653=DIRECTION('center_axis',(0.,0.,1.));
#7654=DIRECTION('ref_axis',(1.,0.,0.));
#7655=DIRECTION('axis',(0.,0.,1.));
#7656=DIRECTION('refdir',(1.,0.,0.));
#7657=DIRECTION('center_axis',(0.,1.,0.));
#7658=DIRECTION('ref_axis',(1.,0.,0.));
#7659=DIRECTION('center_axis',(0.,1.,0.));
#7660=DIRECTION('ref_axis',(1.,0.,0.));
#7661=DIRECTION('',(0.,1.,0.));
#7662=DIRECTION('center_axis',(0.,-1.,0.));
#7663=DIRECTION('ref_axis',(1.,0.,0.));
#7664=DIRECTION('center_axis',(0.,1.,0.));
#7665=DIRECTION('ref_axis',(1.,0.,0.));
#7666=DIRECTION('center_axis',(0.,1.,0.));
#7667=DIRECTION('ref_axis',(1.,0.,0.));
#7668=DIRECTION('',(0.,1.,0.));
#7669=DIRECTION('center_axis',(0.,-1.,0.));
#7670=DIRECTION('ref_axis',(1.,0.,0.));
#7671=DIRECTION('center_axis',(0.,1.,0.));
#7672=DIRECTION('ref_axis',(1.,0.,0.));
#7673=DIRECTION('center_axis',(0.,1.,0.));
#7674=DIRECTION('ref_axis',(1.,0.,0.));
#7675=DIRECTION('',(0.,1.,0.));
#7676=DIRECTION('center_axis',(0.,-1.,0.));
#7677=DIRECTION('ref_axis',(1.,0.,0.));
#7678=DIRECTION('center_axis',(0.,1.,0.));
#7679=DIRECTION('ref_axis',(1.,0.,0.));
#7680=DIRECTION('center_axis',(0.,1.,0.));
#7681=DIRECTION('ref_axis',(1.,0.,0.));
#7682=DIRECTION('',(0.,1.,0.));
#7683=DIRECTION('center_axis',(0.,-1.,0.));
#7684=DIRECTION('ref_axis',(1.,0.,0.));
#7685=DIRECTION('center_axis',(0.,1.,0.));
#7686=DIRECTION('ref_axis',(1.,0.,0.));
#7687=DIRECTION('center_axis',(0.,1.,0.));
#7688=DIRECTION('ref_axis',(1.,0.,0.));
#7689=DIRECTION('',(0.,-1.,0.));
#7690=DIRECTION('center_axis',(0.,-1.,0.));
#7691=DIRECTION('ref_axis',(1.,0.,0.));
#7692=DIRECTION('center_axis',(0.,1.,0.));
#7693=DIRECTION('ref_axis',(1.,0.,0.));
#7694=DIRECTION('center_axis',(0.,-1.,0.));
#7695=DIRECTION('ref_axis',(1.,0.,0.));
#7696=DIRECTION('center_axis',(0.,1.,0.));
#7697=DIRECTION('ref_axis',(1.,0.,0.));
#7698=DIRECTION('',(0.,-1.,0.));
#7699=DIRECTION('center_axis',(0.,-1.,0.));
#7700=DIRECTION('ref_axis',(1.,0.,0.));
#7701=DIRECTION('center_axis',(0.,1.,0.));
#7702=DIRECTION('ref_axis',(1.,0.,0.));
#7703=DIRECTION('center_axis',(0.,1.,0.));
#7704=DIRECTION('ref_axis',(1.,0.,0.));
#7705=DIRECTION('',(0.,-1.,0.));
#7706=DIRECTION('center_axis',(0.,1.,0.));
#7707=DIRECTION('ref_axis',(1.,0.,0.));
#7708=DIRECTION('center_axis',(0.,1.,0.));
#7709=DIRECTION('ref_axis',(1.,0.,0.));
#7710=DIRECTION('center_axis',(0.,1.,0.));
#7711=DIRECTION('ref_axis',(1.,0.,0.));
#7712=DIRECTION('axis',(0.,0.,1.));
#7713=DIRECTION('refdir',(1.,0.,0.));
#7714=DIRECTION('center_axis',(0.,1.,0.));
#7715=DIRECTION('ref_axis',(1.,0.,0.));
#7716=DIRECTION('center_axis',(0.,1.,0.));
#7717=DIRECTION('ref_axis',(1.,0.,0.));
#7718=DIRECTION('',(0.,1.,0.));
#7719=DIRECTION('center_axis',(0.,-1.,0.));
#7720=DIRECTION('ref_axis',(1.,0.,0.));
#7721=DIRECTION('center_axis',(0.,1.,0.));
#7722=DIRECTION('ref_axis',(1.,0.,0.));
#7723=DIRECTION('center_axis',(0.,1.,0.));
#7724=DIRECTION('ref_axis',(1.,0.,0.));
#7725=DIRECTION('',(0.,1.,0.));
#7726=DIRECTION('center_axis',(0.,-1.,0.));
#7727=DIRECTION('ref_axis',(1.,0.,0.));
#7728=DIRECTION('center_axis',(0.,1.,0.));
#7729=DIRECTION('ref_axis',(1.,0.,0.));
#7730=DIRECTION('center_axis',(0.,1.,0.));
#7731=DIRECTION('ref_axis',(1.,0.,0.));
#7732=DIRECTION('',(0.,1.,0.));
#7733=DIRECTION('center_axis',(0.,-1.,0.));
#7734=DIRECTION('ref_axis',(1.,0.,0.));
#7735=DIRECTION('center_axis',(0.,1.,0.));
#7736=DIRECTION('ref_axis',(1.,0.,0.));
#7737=DIRECTION('center_axis',(0.,1.,0.));
#7738=DIRECTION('ref_axis',(1.,0.,0.));
#7739=DIRECTION('',(0.,1.,0.));
#7740=DIRECTION('center_axis',(0.,-1.,0.));
#7741=DIRECTION('ref_axis',(1.,0.,0.));
#7742=DIRECTION('center_axis',(0.,1.,0.));
#7743=DIRECTION('ref_axis',(1.,0.,0.));
#7744=DIRECTION('center_axis',(0.,1.,0.));
#7745=DIRECTION('ref_axis',(1.,0.,0.));
#7746=DIRECTION('',(0.,-1.,0.));
#7747=DIRECTION('center_axis',(0.,1.,0.));
#7748=DIRECTION('ref_axis',(1.,0.,0.));
#7749=DIRECTION('center_axis',(0.,1.,0.));
#7750=DIRECTION('ref_axis',(1.,0.,0.));
#7751=DIRECTION('center_axis',(0.,-1.,0.));
#7752=DIRECTION('ref_axis',(1.,0.,0.));
#7753=DIRECTION('center_axis',(0.,1.,0.));
#7754=DIRECTION('ref_axis',(1.,0.,0.));
#7755=DIRECTION('center_axis',(0.,-1.,0.));
#7756=DIRECTION('ref_axis',(1.,0.,0.));
#7757=DIRECTION('',(0.,-1.,0.));
#7758=DIRECTION('center_axis',(0.,1.,0.));
#7759=DIRECTION('ref_axis',(1.,0.,0.));
#7760=DIRECTION('center_axis',(0.,1.,0.));
#7761=DIRECTION('ref_axis',(1.,0.,0.));
#7762=DIRECTION('',(0.,-1.,0.));
#7763=DIRECTION('center_axis',(0.,1.,0.));
#7764=DIRECTION('ref_axis',(1.,0.,0.));
#7765=DIRECTION('center_axis',(0.,1.,0.));
#7766=DIRECTION('ref_axis',(1.,0.,0.));
#7767=DIRECTION('center_axis',(0.,1.,0.));
#7768=DIRECTION('ref_axis',(1.,0.,0.));
#7769=DIRECTION('axis',(0.,0.,1.));
#7770=DIRECTION('refdir',(1.,0.,0.));
#7771=DIRECTION('center_axis',(0.,0.,1.));
#7772=DIRECTION('ref_axis',(1.,0.,0.));
#7773=DIRECTION('center_axis',(0.,0.,1.));
#7774=DIRECTION('ref_axis',(1.,0.,0.));
#7775=DIRECTION('',(0.,0.,1.));
#7776=DIRECTION('center_axis',(0.,0.,-1.));
#7777=DIRECTION('ref_axis',(1.,0.,0.));
#7778=DIRECTION('center_axis',(0.,0.,1.));
#7779=DIRECTION('ref_axis',(1.,0.,0.));
#7780=DIRECTION('center_axis',(0.,0.,1.));
#7781=DIRECTION('ref_axis',(1.,0.,0.));
#7782=DIRECTION('',(0.,0.,1.));
#7783=DIRECTION('center_axis',(0.,0.,-1.));
#7784=DIRECTION('ref_axis',(1.,0.,0.));
#7785=DIRECTION('center_axis',(0.,1.,0.));
#7786=DIRECTION('ref_axis',(1.,0.,0.));
#7787=DIRECTION('center_axis',(0.,1.,0.));
#7788=DIRECTION('ref_axis',(1.,0.,0.));
#7789=DIRECTION('',(0.,1.,0.));
#7790=DIRECTION('center_axis',(0.,-1.,0.));
#7791=DIRECTION('ref_axis',(1.,0.,0.));
#7792=DIRECTION('center_axis',(0.,1.,0.));
#7793=DIRECTION('ref_axis',(1.,0.,0.));
#7794=DIRECTION('center_axis',(0.,1.,0.));
#7795=DIRECTION('ref_axis',(1.,0.,0.));
#7796=DIRECTION('',(0.,1.,0.));
#7797=DIRECTION('center_axis',(0.,-1.,0.));
#7798=DIRECTION('ref_axis',(1.,0.,0.));
#7799=DIRECTION('center_axis',(0.,1.,0.));
#7800=DIRECTION('ref_axis',(1.,0.,0.));
#7801=DIRECTION('center_axis',(0.,1.,0.));
#7802=DIRECTION('ref_axis',(1.,0.,0.));
#7803=DIRECTION('',(0.,1.,0.));
#7804=DIRECTION('center_axis',(0.,-1.,0.));
#7805=DIRECTION('ref_axis',(1.,0.,0.));
#7806=DIRECTION('center_axis',(0.,1.,0.));
#7807=DIRECTION('ref_axis',(1.,0.,0.));
#7808=DIRECTION('center_axis',(0.,1.,0.));
#7809=DIRECTION('ref_axis',(1.,0.,0.));
#7810=DIRECTION('',(0.,1.,0.));
#7811=DIRECTION('center_axis',(0.,-1.,0.));
#7812=DIRECTION('ref_axis',(1.,0.,0.));
#7813=DIRECTION('center_axis',(0.,1.,0.));
#7814=DIRECTION('ref_axis',(1.,0.,0.));
#7815=DIRECTION('center_axis',(0.,1.,0.));
#7816=DIRECTION('ref_axis',(1.,0.,0.));
#7817=DIRECTION('',(0.,1.,0.));
#7818=DIRECTION('center_axis',(0.,-1.,0.));
#7819=DIRECTION('ref_axis',(1.,0.,0.));
#7820=DIRECTION('center_axis',(0.,0.,1.));
#7821=DIRECTION('ref_axis',(1.,0.,0.));
#7822=DIRECTION('',(0.,1.,0.));
#7823=DIRECTION('',(-1.,0.,0.));
#7824=DIRECTION('',(0.,1.,0.));
#7825=DIRECTION('',(1.,0.,0.));
#7826=DIRECTION('center_axis',(0.,0.,1.));
#7827=DIRECTION('ref_axis',(1.,0.,0.));
#7828=DIRECTION('',(0.,-1.,0.));
#7829=DIRECTION('',(1.,0.,0.));
#7830=DIRECTION('',(0.,1.,0.));
#7831=DIRECTION('',(-1.,0.,0.));
#7832=DIRECTION('center_axis',(-1.,0.,0.));
#7833=DIRECTION('ref_axis',(0.,0.,1.));
#7834=DIRECTION('',(0.,0.,-1.));
#7835=DIRECTION('',(0.,0.,1.));
#7836=DIRECTION('',(0.,1.,0.));
#7837=DIRECTION('center_axis',(1.,0.,0.));
#7838=DIRECTION('ref_axis',(0.,0.,-1.));
#7839=DIRECTION('',(0.,0.,1.));
#7840=DIRECTION('',(0.,1.,0.));
#7841=DIRECTION('',(0.,0.,-1.));
#7842=DIRECTION('center_axis',(0.,-1.,0.));
#7843=DIRECTION('ref_axis',(1.,0.,0.));
#7844=DIRECTION('',(0.,0.,1.));
#7845=DIRECTION('',(1.,0.,0.));
#7846=DIRECTION('',(0.,0.,1.));
#7847=DIRECTION('',(1.,0.,0.));
#7848=DIRECTION('center_axis',(1.,0.,0.));
#7849=DIRECTION('ref_axis',(0.,1.,0.));
#7850=DIRECTION('',(0.,0.,1.));
#7851=DIRECTION('',(0.,1.,0.));
#7852=DIRECTION('center_axis',(0.,1.,0.));
#7853=DIRECTION('ref_axis',(-1.,0.,0.));
#7854=DIRECTION('',(0.,0.,1.));
#7855=DIRECTION('',(-1.,0.,0.));
#7856=DIRECTION('',(-1.,0.,0.));
#7857=DIRECTION('center_axis',(-1.,0.,0.));
#7858=DIRECTION('ref_axis',(0.,-1.,0.));
#7859=DIRECTION('',(0.,-1.,0.));
#7860=DIRECTION('center_axis',(0.,0.,1.));
#7861=DIRECTION('ref_axis',(1.,0.,0.));
#7862=DIRECTION('center_axis',(0.,0.,1.));
#7863=DIRECTION('ref_axis',(1.,0.,0.));
#7864=DIRECTION('axis',(0.,0.,1.));
#7865=DIRECTION('refdir',(1.,0.,0.));
#7866=DIRECTION('center_axis',(0.,1.,0.));
#7867=DIRECTION('ref_axis',(1.,0.,0.));
#7868=DIRECTION('center_axis',(0.,1.,0.));
#7869=DIRECTION('ref_axis',(1.,0.,0.));
#7870=DIRECTION('',(0.,1.,0.));
#7871=DIRECTION('center_axis',(0.,-1.,0.));
#7872=DIRECTION('ref_axis',(1.,0.,0.));
#7873=DIRECTION('center_axis',(0.,1.,0.));
#7874=DIRECTION('ref_axis',(1.,0.,0.));
#7875=DIRECTION('center_axis',(0.,1.,0.));
#7876=DIRECTION('ref_axis',(1.,0.,0.));
#7877=DIRECTION('',(0.,1.,0.));
#7878=DIRECTION('center_axis',(0.,-1.,0.));
#7879=DIRECTION('ref_axis',(1.,0.,0.));
#7880=DIRECTION('center_axis',(0.,1.,0.));
#7881=DIRECTION('ref_axis',(1.,0.,0.));
#7882=DIRECTION('center_axis',(0.,1.,0.));
#7883=DIRECTION('ref_axis',(1.,0.,0.));
#7884=DIRECTION('',(0.,1.,0.));
#7885=DIRECTION('center_axis',(0.,-1.,0.));
#7886=DIRECTION('ref_axis',(1.,0.,0.));
#7887=DIRECTION('center_axis',(0.,1.,0.));
#7888=DIRECTION('ref_axis',(1.,0.,0.));
#7889=DIRECTION('center_axis',(0.,1.,0.));
#7890=DIRECTION('ref_axis',(1.,0.,0.));
#7891=DIRECTION('',(0.,1.,0.));
#7892=DIRECTION('center_axis',(0.,-1.,0.));
#7893=DIRECTION('ref_axis',(1.,0.,0.));
#7894=DIRECTION('center_axis',(0.,1.,0.));
#7895=DIRECTION('ref_axis',(1.,0.,0.));
#7896=DIRECTION('center_axis',(0.,1.,0.));
#7897=DIRECTION('ref_axis',(1.,0.,0.));
#7898=DIRECTION('',(0.,-1.,0.));
#7899=DIRECTION('center_axis',(0.,-1.,0.));
#7900=DIRECTION('ref_axis',(1.,0.,0.));
#7901=DIRECTION('center_axis',(0.,1.,0.));
#7902=DIRECTION('ref_axis',(1.,0.,0.));
#7903=DIRECTION('center_axis',(0.,-1.,0.));
#7904=DIRECTION('ref_axis',(1.,0.,0.));
#7905=DIRECTION('center_axis',(0.,1.,0.));
#7906=DIRECTION('ref_axis',(1.,0.,0.));
#7907=DIRECTION('',(0.,-1.,0.));
#7908=DIRECTION('center_axis',(0.,-1.,0.));
#7909=DIRECTION('ref_axis',(1.,0.,0.));
#7910=DIRECTION('center_axis',(0.,1.,0.));
#7911=DIRECTION('ref_axis',(1.,0.,0.));
#7912=DIRECTION('center_axis',(0.,1.,0.));
#7913=DIRECTION('ref_axis',(1.,0.,0.));
#7914=DIRECTION('',(0.,-1.,0.));
#7915=DIRECTION('center_axis',(0.,1.,0.));
#7916=DIRECTION('ref_axis',(1.,0.,0.));
#7917=DIRECTION('center_axis',(0.,1.,0.));
#7918=DIRECTION('ref_axis',(1.,0.,0.));
#7919=DIRECTION('center_axis',(0.,1.,0.));
#7920=DIRECTION('ref_axis',(1.,0.,0.));
#7921=DIRECTION('axis',(0.,0.,1.));
#7922=DIRECTION('refdir',(1.,0.,0.));
#7923=DIRECTION('center_axis',(0.,1.,0.));
#7924=DIRECTION('ref_axis',(1.,0.,0.));
#7925=DIRECTION('center_axis',(0.,1.,0.));
#7926=DIRECTION('ref_axis',(1.,0.,0.));
#7927=DIRECTION('',(0.,1.,0.));
#7928=DIRECTION('center_axis',(0.,-1.,0.));
#7929=DIRECTION('ref_axis',(1.,0.,0.));
#7930=DIRECTION('center_axis',(0.,1.,0.));
#7931=DIRECTION('ref_axis',(1.,0.,0.));
#7932=DIRECTION('center_axis',(0.,1.,0.));
#7933=DIRECTION('ref_axis',(1.,0.,0.));
#7934=DIRECTION('',(0.,1.,0.));
#7935=DIRECTION('center_axis',(0.,-1.,0.));
#7936=DIRECTION('ref_axis',(1.,0.,0.));
#7937=DIRECTION('center_axis',(0.,1.,0.));
#7938=DIRECTION('ref_axis',(1.,0.,0.));
#7939=DIRECTION('center_axis',(0.,1.,0.));
#7940=DIRECTION('ref_axis',(1.,0.,0.));
#7941=DIRECTION('',(0.,1.,0.));
#7942=DIRECTION('center_axis',(0.,-1.,0.));
#7943=DIRECTION('ref_axis',(1.,0.,0.));
#7944=DIRECTION('center_axis',(0.,1.,0.));
#7945=DIRECTION('ref_axis',(1.,0.,0.));
#7946=DIRECTION('center_axis',(0.,1.,0.));
#7947=DIRECTION('ref_axis',(1.,0.,0.));
#7948=DIRECTION('',(0.,1.,0.));
#7949=DIRECTION('center_axis',(0.,-1.,0.));
#7950=DIRECTION('ref_axis',(1.,0.,0.));
#7951=DIRECTION('center_axis',(0.,1.,0.));
#7952=DIRECTION('ref_axis',(1.,0.,0.));
#7953=DIRECTION('center_axis',(0.,1.,0.));
#7954=DIRECTION('ref_axis',(1.,0.,0.));
#7955=DIRECTION('',(0.,-1.,0.));
#7956=DIRECTION('center_axis',(0.,1.,0.));
#7957=DIRECTION('ref_axis',(1.,0.,0.));
#7958=DIRECTION('center_axis',(0.,1.,0.));
#7959=DIRECTION('ref_axis',(1.,0.,0.));
#7960=DIRECTION('center_axis',(0.,-1.,0.));
#7961=DIRECTION('ref_axis',(1.,0.,0.));
#7962=DIRECTION('center_axis',(0.,1.,0.));
#7963=DIRECTION('ref_axis',(1.,0.,0.));
#7964=DIRECTION('center_axis',(0.,-1.,0.));
#7965=DIRECTION('ref_axis',(1.,0.,0.));
#7966=DIRECTION('',(0.,-1.,0.));
#7967=DIRECTION('center_axis',(0.,1.,0.));
#7968=DIRECTION('ref_axis',(1.,0.,0.));
#7969=DIRECTION('center_axis',(0.,1.,0.));
#7970=DIRECTION('ref_axis',(1.,0.,0.));
#7971=DIRECTION('',(0.,-1.,0.));
#7972=DIRECTION('center_axis',(0.,1.,0.));
#7973=DIRECTION('ref_axis',(1.,0.,0.));
#7974=DIRECTION('center_axis',(0.,1.,0.));
#7975=DIRECTION('ref_axis',(1.,0.,0.));
#7976=DIRECTION('center_axis',(0.,1.,0.));
#7977=DIRECTION('ref_axis',(1.,0.,0.));
#7978=DIRECTION('axis',(0.,0.,1.));
#7979=DIRECTION('refdir',(1.,0.,0.));
#7980=DIRECTION('center_axis',(0.,0.,1.));
#7981=DIRECTION('ref_axis',(1.,0.,0.));
#7982=DIRECTION('center_axis',(0.,0.,1.));
#7983=DIRECTION('ref_axis',(1.,0.,0.));
#7984=DIRECTION('',(0.,0.,1.));
#7985=DIRECTION('center_axis',(0.,0.,-1.));
#7986=DIRECTION('ref_axis',(1.,0.,0.));
#7987=DIRECTION('center_axis',(0.,0.,1.));
#7988=DIRECTION('ref_axis',(1.,0.,0.));
#7989=DIRECTION('center_axis',(0.,0.,1.));
#7990=DIRECTION('ref_axis',(1.,0.,0.));
#7991=DIRECTION('center_axis',(0.,0.,1.));
#7992=DIRECTION('ref_axis',(1.,0.,0.));
#7993=DIRECTION('',(0.,0.,1.));
#7994=DIRECTION('center_axis',(0.,0.,-1.));
#7995=DIRECTION('ref_axis',(1.,0.,0.));
#7996=DIRECTION('center_axis',(0.,0.,1.));
#7997=DIRECTION('ref_axis',(1.,0.,0.));
#7998=DIRECTION('center_axis',(0.,0.,1.));
#7999=DIRECTION('ref_axis',(1.,0.,0.));
#8000=DIRECTION('center_axis',(0.,0.,1.));
#8001=DIRECTION('ref_axis',(1.,0.,0.));
#8002=DIRECTION('',(0.,0.,1.));
#8003=DIRECTION('center_axis',(0.,0.,-1.));
#8004=DIRECTION('ref_axis',(1.,0.,0.));
#8005=DIRECTION('center_axis',(0.,0.,1.));
#8006=DIRECTION('ref_axis',(1.,0.,0.));
#8007=DIRECTION('center_axis',(0.,0.,1.));
#8008=DIRECTION('ref_axis',(1.,0.,0.));
#8009=DIRECTION('center_axis',(0.,0.,1.));
#8010=DIRECTION('ref_axis',(1.,0.,0.));
#8011=DIRECTION('',(0.,0.,1.));
#8012=DIRECTION('center_axis',(0.,0.,-1.));
#8013=DIRECTION('ref_axis',(1.,0.,0.));
#8014=DIRECTION('center_axis',(0.,0.,1.));
#8015=DIRECTION('ref_axis',(1.,0.,0.));
#8016=DIRECTION('center_axis',(0.,0.,1.));
#8017=DIRECTION('ref_axis',(1.,0.,0.));
#8018=DIRECTION('center_axis',(0.,0.,1.));
#8019=DIRECTION('ref_axis',(1.,0.,0.));
#8020=DIRECTION('',(0.,0.,1.));
#8021=DIRECTION('center_axis',(0.,0.,-1.));
#8022=DIRECTION('ref_axis',(1.,0.,0.));
#8023=DIRECTION('center_axis',(0.,0.,1.));
#8024=DIRECTION('ref_axis',(1.,0.,0.));
#8025=DIRECTION('center_axis',(0.,0.,1.));
#8026=DIRECTION('ref_axis',(1.,0.,0.));
#8027=DIRECTION('center_axis',(0.,0.,1.));
#8028=DIRECTION('ref_axis',(1.,0.,0.));
#8029=DIRECTION('center_axis',(0.,0.,1.));
#8030=DIRECTION('ref_axis',(1.,0.,0.));
#8031=DIRECTION('',(0.,0.,1.));
#8032=DIRECTION('center_axis',(0.,0.,1.));
#8033=DIRECTION('ref_axis',(1.,0.,0.));
#8034=DIRECTION('center_axis',(0.,0.,1.));
#8035=DIRECTION('ref_axis',(1.,0.,0.));
#8036=DIRECTION('',(0.,0.,1.));
#8037=DIRECTION('center_axis',(0.,0.,-1.));
#8038=DIRECTION('ref_axis',(1.,0.,0.));
#8039=DIRECTION('center_axis',(0.,0.,1.));
#8040=DIRECTION('ref_axis',(1.,0.,0.));
#8041=DIRECTION('center_axis',(0.,0.,1.));
#8042=DIRECTION('ref_axis',(1.,0.,0.));
#8043=DIRECTION('center_axis',(0.,0.,1.));
#8044=DIRECTION('ref_axis',(1.,0.,0.));
#8045=DIRECTION('center_axis',(0.,0.,1.));
#8046=DIRECTION('ref_axis',(1.,0.,0.));
#8047=DIRECTION('',(0.,0.,1.));
#8048=DIRECTION('center_axis',(0.,0.,1.));
#8049=DIRECTION('ref_axis',(1.,0.,0.));
#8050=DIRECTION('center_axis',(0.,0.,1.));
#8051=DIRECTION('ref_axis',(1.,0.,0.));
#8052=DIRECTION('',(0.,0.,1.));
#8053=DIRECTION('center_axis',(0.,0.,-1.));
#8054=DIRECTION('ref_axis',(1.,0.,0.));
#8055=DIRECTION('center_axis',(0.,0.,1.));
#8056=DIRECTION('ref_axis',(1.,0.,0.));
#8057=DIRECTION('center_axis',(0.,0.,1.));
#8058=DIRECTION('ref_axis',(1.,0.,0.));
#8059=DIRECTION('center_axis',(0.,0.,1.));
#8060=DIRECTION('ref_axis',(1.,0.,0.));
#8061=DIRECTION('center_axis',(0.,0.,1.));
#8062=DIRECTION('ref_axis',(1.,0.,0.));
#8063=DIRECTION('',(0.,0.,1.));
#8064=DIRECTION('center_axis',(0.,0.,-1.));
#8065=DIRECTION('ref_axis',(-1.,0.,0.));
#8066=DIRECTION('',(1.,0.,0.));
#8067=DIRECTION('',(0.,1.,0.));
#8068=DIRECTION('',(-1.,0.,0.));
#8069=DIRECTION('',(0.,1.,0.));
#8070=DIRECTION('',(1.,0.,0.));
#8071=DIRECTION('',(0.,1.,0.));
#8072=DIRECTION('',(-1.,0.,0.));
#8073=DIRECTION('',(0.,1.,0.));
#8074=DIRECTION('',(1.,0.,0.));
#8075=DIRECTION('',(0.,1.,0.));
#8076=DIRECTION('',(-1.,0.,0.));
#8077=DIRECTION('',(0.,-1.,0.));
#8078=DIRECTION('center_axis',(0.,1.,0.));
#8079=DIRECTION('ref_axis',(0.,0.,1.));
#8080=DIRECTION('',(1.,0.,0.));
#8081=DIRECTION('',(0.,0.,-1.));
#8082=DIRECTION('',(0.,0.,1.));
#8083=DIRECTION('center_axis',(0.,1.,0.));
#8084=DIRECTION('ref_axis',(1.,0.,0.));
#8085=DIRECTION('',(-1.,0.,0.));
#8086=DIRECTION('',(0.,0.,-1.));
#8087=DIRECTION('',(0.,0.,1.));
#8088=DIRECTION('center_axis',(-1.,0.,0.));
#8089=DIRECTION('ref_axis',(0.,0.,1.));
#8090=DIRECTION('',(0.,0.,1.));
#8091=DIRECTION('',(0.,1.,0.));
#8092=DIRECTION('',(0.,0.,-1.));
#8093=DIRECTION('center_axis',(0.,1.,0.));
#8094=DIRECTION('ref_axis',(0.,0.,1.));
#8095=DIRECTION('',(0.,0.,-1.));
#8096=DIRECTION('',(-1.,0.,0.));
#8097=DIRECTION('center_axis',(0.,0.,-1.));
#8098=DIRECTION('ref_axis',(-1.,0.,0.));
#8099=DIRECTION('',(1.,0.,0.));
#8100=DIRECTION('',(0.,1.,0.));
#8101=DIRECTION('center_axis',(1.,0.,0.));
#8102=DIRECTION('ref_axis',(0.,0.,-1.));
#8103=DIRECTION('',(0.,0.,1.));
#8104=DIRECTION('',(0.,1.,0.));
#8105=DIRECTION('center_axis',(0.,1.,0.));
#8106=DIRECTION('ref_axis',(1.,0.,0.));
#8107=DIRECTION('center_axis',(1.,0.,0.));
#8108=DIRECTION('ref_axis',(0.,1.,0.));
#8109=DIRECTION('',(0.,0.,1.));
#8110=DIRECTION('',(0.,1.,0.));
#8111=DIRECTION('',(0.,0.,1.));
#8112=DIRECTION('center_axis',(0.,-1.,0.));
#8113=DIRECTION('ref_axis',(1.,0.,0.));
#8114=DIRECTION('',(0.,0.,1.));
#8115=DIRECTION('',(1.,0.,0.));
#8116=DIRECTION('center_axis',(0.,1.,0.));
#8117=DIRECTION('ref_axis',(-1.,0.,0.));
#8118=DIRECTION('',(-1.,0.,0.));
#8119=DIRECTION('',(0.,0.,1.));
#8120=DIRECTION('center_axis',(-1.,0.,0.));
#8121=DIRECTION('ref_axis',(0.,-1.,0.));
#8122=DIRECTION('',(0.,-1.,0.));
#8123=DIRECTION('',(0.,1.,0.));
#8124=DIRECTION('center_axis',(0.,0.,1.));
#8125=DIRECTION('ref_axis',(1.,0.,0.));
#8126=DIRECTION('center_axis',(0.,0.,1.));
#8127=DIRECTION('ref_axis',(1.,0.,0.));
#8128=DIRECTION('axis',(0.,0.,1.));
#8129=DIRECTION('refdir',(1.,0.,0.));
#8130=DIRECTION('center_axis',(0.,0.,1.));
#8131=DIRECTION('ref_axis',(1.,0.,0.));
#8132=DIRECTION('center_axis',(0.,0.,1.));
#8133=DIRECTION('ref_axis',(1.,0.,0.));
#8134=DIRECTION('',(0.,0.,1.));
#8135=DIRECTION('center_axis',(0.,0.,-1.));
#8136=DIRECTION('ref_axis',(1.,0.,0.));
#8137=DIRECTION('center_axis',(0.,0.,1.));
#8138=DIRECTION('ref_axis',(1.,0.,0.));
#8139=DIRECTION('center_axis',(0.,0.,1.));
#8140=DIRECTION('ref_axis',(1.,0.,0.));
#8141=DIRECTION('',(0.,0.,1.));
#8142=DIRECTION('center_axis',(0.,0.,-1.));
#8143=DIRECTION('ref_axis',(1.,0.,0.));
#8144=DIRECTION('center_axis',(0.,0.,1.));
#8145=DIRECTION('ref_axis',(1.,0.,0.));
#8146=DIRECTION('center_axis',(0.,0.,1.));
#8147=DIRECTION('ref_axis',(1.,0.,0.));
#8148=DIRECTION('',(0.,0.,1.));
#8149=DIRECTION('center_axis',(0.,0.,-1.));
#8150=DIRECTION('ref_axis',(1.,0.,0.));
#8151=DIRECTION('center_axis',(0.,0.,1.));
#8152=DIRECTION('ref_axis',(1.,0.,0.));
#8153=DIRECTION('center_axis',(0.,0.,1.));
#8154=DIRECTION('ref_axis',(1.,0.,0.));
#8155=DIRECTION('',(0.,0.,1.));
#8156=DIRECTION('center_axis',(0.,0.,-1.));
#8157=DIRECTION('ref_axis',(1.,0.,0.));
#8158=DIRECTION('center_axis',(0.,0.,1.));
#8159=DIRECTION('ref_axis',(1.,0.,0.));
#8160=DIRECTION('center_axis',(0.,0.,1.));
#8161=DIRECTION('ref_axis',(1.,0.,0.));
#8162=DIRECTION('',(0.,0.,-1.));
#8163=DIRECTION('center_axis',(0.,0.,1.));
#8164=DIRECTION('ref_axis',(1.,0.,0.));
#8165=DIRECTION('center_axis',(0.,0.,1.));
#8166=DIRECTION('ref_axis',(1.,0.,0.));
#8167=DIRECTION('center_axis',(0.,0.,-1.));
#8168=DIRECTION('ref_axis',(1.,0.,0.));
#8169=DIRECTION('center_axis',(0.,0.,1.));
#8170=DIRECTION('ref_axis',(1.,0.,0.));
#8171=DIRECTION('center_axis',(0.,0.,-1.));
#8172=DIRECTION('ref_axis',(1.,0.,0.));
#8173=DIRECTION('',(0.,0.,-1.));
#8174=DIRECTION('center_axis',(0.,0.,1.));
#8175=DIRECTION('ref_axis',(1.,0.,0.));
#8176=DIRECTION('center_axis',(0.,0.,1.));
#8177=DIRECTION('ref_axis',(1.,0.,0.));
#8178=DIRECTION('',(0.,0.,-1.));
#8179=DIRECTION('center_axis',(0.,0.,1.));
#8180=DIRECTION('ref_axis',(1.,0.,0.));
#8181=DIRECTION('center_axis',(0.,0.,1.));
#8182=DIRECTION('ref_axis',(1.,0.,0.));
#8183=DIRECTION('center_axis',(0.,0.,1.));
#8184=DIRECTION('ref_axis',(1.,0.,0.));
#8185=DIRECTION('axis',(0.,0.,1.));
#8186=DIRECTION('refdir',(1.,0.,0.));
#8187=DIRECTION('center_axis',(-0.00013450227597807,0.999117050244768,0.042013114849203));
#8188=DIRECTION('ref_axis',(5.65585335115278E-6,-0.0420131144685042,0.999117059298192));
#8189=DIRECTION('center_axis',(0.000134502259908405,0.999117050228794,0.0420131152291186));
#8190=DIRECTION('ref_axis',(-0.474109261639291,0.0370548329511252,-0.879685936788131));
#8191=DIRECTION('center_axis',(0.000134502259908405,0.999117050228794,0.0420131152291186));
#8192=DIRECTION('ref_axis',(-0.474109261639291,0.0370548329511252,-0.879685936788131));
#8193=DIRECTION('center_axis',(-0.00013450227597807,0.999117050244768,0.042013114849203));
#8194=DIRECTION('ref_axis',(5.65585335115278E-6,-0.0420131144685042,0.999117059298193));
#8195=DIRECTION('axis',(0.,0.,1.));
#8196=DIRECTION('refdir',(1.,0.,0.));
#8197=DIRECTION('axis',(0.,0.,1.));
#8198=DIRECTION('refdir',(1.,0.,0.));
#8199=DIRECTION('center_axis',(0.,-1.,0.));
#8200=DIRECTION('ref_axis',(0.,0.,-1.));
#8201=DIRECTION('center_axis',(0.,-1.,0.));
#8202=DIRECTION('ref_axis',(1.,0.,0.));
#8203=DIRECTION('center_axis',(0.,-1.,0.));
#8204=DIRECTION('ref_axis',(1.,0.,0.));
#8205=DIRECTION('center_axis',(1.,0.,1.22464679914735E-16));
#8206=DIRECTION('ref_axis',(-1.22464679914735E-16,0.,1.));
#8207=DIRECTION('center_axis',(0.,1.,0.));
#8208=DIRECTION('ref_axis',(1.,0.,0.));
#8209=DIRECTION('center_axis',(0.,1.,0.));
#8210=DIRECTION('ref_axis',(1.,0.,0.));
#8211=DIRECTION('center_axis',(0.,-1.,0.));
#8212=DIRECTION('ref_axis',(1.,0.,0.));
#8213=DIRECTION('',(0.,1.,0.));
#8214=DIRECTION('center_axis',(0.,-1.,0.));
#8215=DIRECTION('ref_axis',(1.,0.,0.));
#8216=DIRECTION('center_axis',(0.,-1.,0.));
#8217=DIRECTION('ref_axis',(1.,0.,0.));
#8218=DIRECTION('center_axis',(0.,-1.,0.));
#8219=DIRECTION('ref_axis',(1.,0.,0.));
#8220=DIRECTION('',(0.,1.,0.));
#8221=DIRECTION('center_axis',(0.,-1.,0.));
#8222=DIRECTION('ref_axis',(1.,0.,0.));
#8223=DIRECTION('center_axis',(0.,1.,0.));
#8224=DIRECTION('ref_axis',(1.,0.,0.));
#8225=DIRECTION('',(-0.707106781186548,0.707106781186547,-8.65956056235493E-17));
#8226=DIRECTION('center_axis',(0.,-1.,0.));
#8227=DIRECTION('ref_axis',(1.,0.,0.));
#8228=DIRECTION('center_axis',(0.,1.,0.));
#8229=DIRECTION('ref_axis',(0.,0.,1.));
#8230=DIRECTION('center_axis',(0.,-1.,0.));
#8231=DIRECTION('ref_axis',(1.,0.,0.));
#8232=DIRECTION('center_axis',(0.,-1.,0.));
#8233=DIRECTION('ref_axis',(1.,0.,0.));
#8234=DIRECTION('',(0.,1.,0.));
#8235=DIRECTION('center_axis',(0.,-1.,0.));
#8236=DIRECTION('ref_axis',(0.,0.,-1.));
#8237=DIRECTION('center_axis',(0.,-1.,0.));
#8238=DIRECTION('ref_axis',(1.,0.,0.));
#8239=DIRECTION('center_axis',(0.,-1.,0.));
#8240=DIRECTION('ref_axis',(1.,0.,0.));
#8241=DIRECTION('',(0.707106781186548,0.707106781186547,8.65956056235493E-17));
#8242=DIRECTION('axis',(0.,0.,1.));
#8243=DIRECTION('refdir',(1.,0.,0.));
#8244=DIRECTION('center_axis',(0.,-1.,0.));
#8245=DIRECTION('ref_axis',(0.,0.,-1.));
#8246=DIRECTION('center_axis',(0.,-1.,0.));
#8247=DIRECTION('ref_axis',(1.,0.,0.));
#8248=DIRECTION('center_axis',(0.,-1.,0.));
#8249=DIRECTION('ref_axis',(1.,0.,0.));
#8250=DIRECTION('center_axis',(1.,0.,1.22464679914735E-16));
#8251=DIRECTION('ref_axis',(-1.22464679914735E-16,0.,1.));
#8252=DIRECTION('center_axis',(0.,1.,0.));
#8253=DIRECTION('ref_axis',(1.,0.,0.));
#8254=DIRECTION('center_axis',(0.,1.,0.));
#8255=DIRECTION('ref_axis',(1.,0.,0.));
#8256=DIRECTION('center_axis',(0.,-1.,0.));
#8257=DIRECTION('ref_axis',(1.,0.,0.));
#8258=DIRECTION('center_axis',(0.,-1.,0.));
#8259=DIRECTION('ref_axis',(1.,0.,0.));
#8260=DIRECTION('',(0.,1.,0.));
#8261=DIRECTION('center_axis',(0.,1.,0.));
#8262=DIRECTION('ref_axis',(0.,0.,1.));
#8263=DIRECTION('center_axis',(0.,-1.,0.));
#8264=DIRECTION('ref_axis',(1.,0.,0.));
#8265=DIRECTION('center_axis',(0.,-1.,0.));
#8266=DIRECTION('ref_axis',(1.,0.,0.));
#8267=DIRECTION('center_axis',(0.,-1.,0.));
#8268=DIRECTION('ref_axis',(1.,0.,0.));
#8269=DIRECTION('center_axis',(0.,-1.,0.));
#8270=DIRECTION('ref_axis',(1.,0.,0.));
#8271=DIRECTION('',(0.707106781186548,0.707106781186547,8.65956056235494E-17));
#8272=DIRECTION('center_axis',(0.,-1.,0.));
#8273=DIRECTION('ref_axis',(1.,0.,0.));
#8274=DIRECTION('center_axis',(0.,-1.,0.));
#8275=DIRECTION('ref_axis',(1.,0.,0.));
#8276=DIRECTION('',(0.,1.,0.));
#8277=DIRECTION('center_axis',(0.,1.,0.));
#8278=DIRECTION('ref_axis',(1.,0.,0.));
#8279=DIRECTION('center_axis',(0.,-1.,0.));
#8280=DIRECTION('ref_axis',(1.,0.,0.));
#8281=DIRECTION('',(-0.707106781186548,0.707106781186547,-8.65956056235494E-17));
#8282=DIRECTION('center_axis',(0.,-1.,0.));
#8283=DIRECTION('ref_axis',(0.,0.,-1.));
#8284=DIRECTION('center_axis',(0.,-1.,0.));
#8285=DIRECTION('ref_axis',(1.,0.,0.));
#8286=DIRECTION('',(0.,1.,0.));
#8287=DIRECTION('axis',(0.,0.,1.));
#8288=DIRECTION('refdir',(1.,0.,0.));
#8289=DIRECTION('center_axis',(0.,0.,1.));
#8290=DIRECTION('ref_axis',(1.,0.,0.));
#8291=DIRECTION('center_axis',(1.22464679914735E-16,-1.,0.));
#8292=DIRECTION('ref_axis',(-1.,-1.22464679914735E-16,0.));
#8293=DIRECTION('center_axis',(0.78183148246803,0.,0.623489801858733));
#8294=DIRECTION('ref_axis',(0.623489801858734,0.,-0.78183148246803));
#8295=DIRECTION('center_axis',(7.63554790147315E-17,-1.,-9.57467422477103E-17));
#8296=DIRECTION('ref_axis',(-0.623489801858734,-1.22464679914735E-16,0.78183148246803));
#8297=DIRECTION('center_axis',(0.974927912181824,0.,-0.222520933956314));
#8298=DIRECTION('ref_axis',(-0.222520933956314,0.,-0.974927912181824));
#8299=DIRECTION('center_axis',(-2.7250954951288E-17,-1.,-1.19394234705288E-16));
#8300=DIRECTION('ref_axis',(0.222520933956314,-1.22464679914735E-16,0.974927912181824));
#8301=DIRECTION('center_axis',(0.433883739117558,0.,-0.900968867902419));
#8302=DIRECTION('ref_axis',(-0.900968867902419,0.,-0.433883739117558));
#8303=DIRECTION('center_axis',(-1.10336864020811E-16,-1.,-5.31354332312403E-17));
#8304=DIRECTION('ref_axis',(0.900968867902419,-1.22464679914735E-16,0.433883739117558));
#8305=DIRECTION('center_axis',(-0.433883739117558,0.,-0.900968867902419));
#8306=DIRECTION('ref_axis',(-0.900968867902419,0.,0.433883739117558));
#8307=DIRECTION('center_axis',(-1.10336864020811E-16,-1.,5.31354332312403E-17));
#8308=DIRECTION('ref_axis',(0.900968867902419,-1.22464679914735E-16,-0.433883739117558));
#8309=DIRECTION('center_axis',(-0.974927912181824,0.,-0.222520933956314));
#8310=DIRECTION('ref_axis',(-0.222520933956315,0.,0.974927912181824));
#8311=DIRECTION('center_axis',(-2.7250954951288E-17,-1.,1.19394234705288E-16));
#8312=DIRECTION('ref_axis',(0.222520933956315,-1.22464679914735E-16,-0.974927912181824));
#8313=DIRECTION('center_axis',(-0.78183148246803,0.,0.623489801858734));
#8314=DIRECTION('ref_axis',(0.623489801858733,0.,0.78183148246803));
#8315=DIRECTION('center_axis',(7.63554790147315E-17,-1.,9.57467422477103E-17));
#8316=DIRECTION('ref_axis',(-0.623489801858733,-1.22464679914735E-16,-0.78183148246803));
#8317=DIRECTION('axis',(0.,0.,1.));
#8318=DIRECTION('refdir',(1.,0.,0.));
#8319=DIRECTION('center_axis',(0.,0.,1.));
#8320=DIRECTION('ref_axis',(1.,0.,0.));
#8321=DIRECTION('center_axis',(0.,-1.,0.));
#8322=DIRECTION('ref_axis',(0.,0.,-1.));
#8323=DIRECTION('center_axis',(0.,-1.,0.));
#8324=DIRECTION('ref_axis',(0.,0.,-1.));
#8325=DIRECTION('center_axis',(0.,1.,0.));
#8326=DIRECTION('ref_axis',(1.,0.,0.));
#8327=DIRECTION('center_axis',(0.,1.,0.));
#8328=DIRECTION('ref_axis',(1.,0.,0.));
#8329=DIRECTION('center_axis',(0.,1.,0.));
#8330=DIRECTION('ref_axis',(1.,0.,0.));
#8331=DIRECTION('center_axis',(0.,1.,0.));
#8332=DIRECTION('ref_axis',(1.,0.,0.));
#8333=DIRECTION('',(0.,-1.,0.));
#8334=DIRECTION('center_axis',(0.,-1.,0.));
#8335=DIRECTION('ref_axis',(1.,0.,0.));
#8336=DIRECTION('center_axis',(0.,1.,0.));
#8337=DIRECTION('ref_axis',(1.,0.,0.));
#8338=DIRECTION('center_axis',(0.,1.,0.));
#8339=DIRECTION('ref_axis',(1.,0.,0.));
#8340=DIRECTION('center_axis',(0.,1.,0.));
#8341=DIRECTION('ref_axis',(1.,0.,0.));
#8342=DIRECTION('center_axis',(0.,1.,0.));
#8343=DIRECTION('ref_axis',(1.,0.,0.));
#8344=DIRECTION('center_axis',(0.,1.,0.));
#8345=DIRECTION('ref_axis',(1.,0.,0.));
#8346=DIRECTION('center_axis',(0.,1.,0.));
#8347=DIRECTION('ref_axis',(1.,0.,0.));
#8348=DIRECTION('center_axis',(0.,-1.,0.));
#8349=DIRECTION('ref_axis',(1.,0.,0.));
#8350=DIRECTION('center_axis',(0.,-1.,0.));
#8351=DIRECTION('ref_axis',(0.,0.,-1.));
#8352=DIRECTION('center_axis',(8.96625347776458E-17,0.,1.));
#8353=DIRECTION('ref_axis',(1.,0.,0.));
#8354=DIRECTION('center_axis',(0.,-1.,0.));
#8355=DIRECTION('ref_axis',(0.,0.,-1.));
#8356=DIRECTION('center_axis',(0.,1.,0.));
#8357=DIRECTION('ref_axis',(1.,0.,0.));
#8358=DIRECTION('center_axis',(0.,-1.,0.));
#8359=DIRECTION('ref_axis',(1.,0.,0.));
#8360=DIRECTION('center_axis',(0.,-1.,0.));
#8361=DIRECTION('ref_axis',(0.,0.,-1.));
#8362=DIRECTION('center_axis',(0.,0.,1.));
#8363=DIRECTION('ref_axis',(1.,0.,0.));
#8364=DIRECTION('center_axis',(0.,-1.,0.));
#8365=DIRECTION('ref_axis',(0.,0.,-1.));
#8366=DIRECTION('center_axis',(0.,1.,0.));
#8367=DIRECTION('ref_axis',(1.,0.,0.));
#8368=DIRECTION('center_axis',(0.,-1.,0.));
#8369=DIRECTION('ref_axis',(1.,0.,0.));
#8370=DIRECTION('center_axis',(0.,-1.,0.));
#8371=DIRECTION('ref_axis',(1.,0.,0.));
#8372=DIRECTION('center_axis',(0.,-1.,0.));
#8373=DIRECTION('ref_axis',(0.,0.,-1.));
#8374=DIRECTION('center_axis',(0.,0.,1.));
#8375=DIRECTION('ref_axis',(1.,0.,0.));
#8376=DIRECTION('center_axis',(0.,-1.,0.));
#8377=DIRECTION('ref_axis',(0.,0.,-1.));
#8378=DIRECTION('center_axis',(0.,1.,0.));
#8379=DIRECTION('ref_axis',(1.,0.,0.));
#8380=DIRECTION('center_axis',(0.,-1.,0.));
#8381=DIRECTION('ref_axis',(1.,0.,0.));
#8382=DIRECTION('center_axis',(0.,-1.,0.));
#8383=DIRECTION('ref_axis',(0.,0.,-1.));
#8384=DIRECTION('center_axis',(8.96625347776458E-17,0.,1.));
#8385=DIRECTION('ref_axis',(1.,0.,0.));
#8386=DIRECTION('center_axis',(0.,-1.,0.));
#8387=DIRECTION('ref_axis',(0.,0.,-1.));
#8388=DIRECTION('center_axis',(0.,1.,0.));
#8389=DIRECTION('ref_axis',(1.,0.,0.));
#8390=DIRECTION('center_axis',(0.,-1.,0.));
#8391=DIRECTION('ref_axis',(1.,0.,0.));
#8392=DIRECTION('center_axis',(0.,-1.,0.));
#8393=DIRECTION('ref_axis',(0.,0.,-1.));
#8394=DIRECTION('center_axis',(0.,0.,1.));
#8395=DIRECTION('ref_axis',(1.,0.,0.));
#8396=DIRECTION('center_axis',(0.,-1.,0.));
#8397=DIRECTION('ref_axis',(0.,0.,-1.));
#8398=DIRECTION('center_axis',(0.,1.,0.));
#8399=DIRECTION('ref_axis',(1.,0.,0.));
#8400=DIRECTION('center_axis',(0.,1.,0.));
#8401=DIRECTION('ref_axis',(1.,0.,0.));
#8402=DIRECTION('',(0.,1.,0.));
#8403=DIRECTION('center_axis',(0.,-1.,0.));
#8404=DIRECTION('ref_axis',(1.,0.,0.));
#8405=DIRECTION('center_axis',(0.,-1.,0.));
#8406=DIRECTION('ref_axis',(1.,0.,0.));
#8407=DIRECTION('center_axis',(0.,1.,0.));
#8408=DIRECTION('ref_axis',(1.,0.,0.));
#8409=DIRECTION('center_axis',(0.,-1.,0.));
#8410=DIRECTION('ref_axis',(0.,0.,-1.));
#8411=DIRECTION('center_axis',(0.,0.,1.));
#8412=DIRECTION('ref_axis',(1.,0.,0.));
#8413=DIRECTION('center_axis',(0.,-1.,0.));
#8414=DIRECTION('ref_axis',(0.,0.,-1.));
#8415=DIRECTION('center_axis',(0.,-1.,0.));
#8416=DIRECTION('ref_axis',(-1.,0.,0.));
#8417=DIRECTION('center_axis',(0.,1.,0.));
#8418=DIRECTION('ref_axis',(1.,0.,0.));
#8419=DIRECTION('axis',(0.,0.,1.));
#8420=DIRECTION('refdir',(1.,0.,0.));
#8421=DIRECTION('center_axis',(0.,1.,0.));
#8422=DIRECTION('ref_axis',(0.,0.,1.));
#8423=DIRECTION('center_axis',(0.,-1.,0.));
#8424=DIRECTION('ref_axis',(1.,0.,0.));
#8425=DIRECTION('center_axis',(0.,-1.,0.));
#8426=DIRECTION('ref_axis',(1.,0.,0.));
#8427=DIRECTION('center_axis',(0.,-1.,0.));
#8428=DIRECTION('ref_axis',(1.,0.,0.));
#8429=DIRECTION('center_axis',(0.,-1.,0.));
#8430=DIRECTION('ref_axis',(1.,0.,0.));
#8431=DIRECTION('',(0.,1.,0.));
#8432=DIRECTION('center_axis',(0.,-1.,0.));
#8433=DIRECTION('ref_axis',(0.,0.,-1.));
#8434=DIRECTION('center_axis',(0.,-1.,0.));
#8435=DIRECTION('ref_axis',(1.,0.,0.));
#8436=DIRECTION('center_axis',(0.,-1.,0.));
#8437=DIRECTION('ref_axis',(1.,0.,0.));
#8438=DIRECTION('',(0.,1.,0.));
#8439=DIRECTION('center_axis',(0.,1.,0.));
#8440=DIRECTION('ref_axis',(0.,0.,1.));
#8441=DIRECTION('center_axis',(0.,-1.,0.));
#8442=DIRECTION('ref_axis',(1.,0.,0.));
#8443=DIRECTION('center_axis',(0.,-1.,0.));
#8444=DIRECTION('ref_axis',(1.,0.,0.));
#8445=DIRECTION('center_axis',(0.,-1.,0.));
#8446=DIRECTION('ref_axis',(1.,0.,0.));
#8447=DIRECTION('center_axis',(0.,-1.,0.));
#8448=DIRECTION('ref_axis',(1.,0.,0.));
#8449=DIRECTION('',(0.,1.,0.));
#8450=DIRECTION('center_axis',(0.,-1.,0.));
#8451=DIRECTION('ref_axis',(0.,0.,-1.));
#8452=DIRECTION('center_axis',(0.,-1.,0.));
#8453=DIRECTION('ref_axis',(1.,0.,0.));
#8454=DIRECTION('center_axis',(0.,-1.,0.));
#8455=DIRECTION('ref_axis',(1.,0.,0.));
#8456=DIRECTION('',(0.,1.,0.));
#8457=DIRECTION('',(0.,0.,1.));
#8458=DIRECTION('',(1.,0.,0.));
#8459=DIRECTION('',(0.,0.,1.));
#8460=DIRECTION('',(1.,0.,0.));
#8461=DIRECTION('',(0.,0.,1.));
#8462=DIRECTION('',(1.,0.,0.));
#8463=DIRECTION('',(0.,0.,1.));
#8464=DIRECTION('',(1.,0.,0.));
#8465=DIRECTION('',(0.,0.,1.));
#8466=DIRECTION('',(1.,0.,0.));
#8467=DIRECTION('axis',(0.,0.,1.));
#8468=DIRECTION('refdir',(1.,0.,0.));
#8469=DIRECTION('center_axis',(0.,1.,0.));
#8470=DIRECTION('ref_axis',(0.,0.,1.));
#8471=DIRECTION('center_axis',(0.,-1.,0.));
#8472=DIRECTION('ref_axis',(1.,0.,0.));
#8473=DIRECTION('center_axis',(0.,-1.,0.));
#8474=DIRECTION('ref_axis',(1.,0.,0.));
#8475=DIRECTION('center_axis',(0.,-1.,0.));
#8476=DIRECTION('ref_axis',(1.,0.,0.));
#8477=DIRECTION('',(0.707106781186548,0.707106781186547,8.65956056235493E-17));
#8478=DIRECTION('center_axis',(0.,-1.,0.));
#8479=DIRECTION('ref_axis',(1.,0.,0.));
#8480=DIRECTION('center_axis',(0.,-1.,0.));
#8481=DIRECTION('ref_axis',(1.,0.,0.));
#8482=DIRECTION('',(0.,1.,0.));
#8483=DIRECTION('center_axis',(0.,1.,0.));
#8484=DIRECTION('ref_axis',(1.,0.,0.));
#8485=DIRECTION('center_axis',(0.,-1.,0.));
#8486=DIRECTION('ref_axis',(1.,0.,0.));
#8487=DIRECTION('',(-0.707106781186547,0.707106781186548,-8.65956056235493E-17));
#8488=DIRECTION('center_axis',(0.,-1.,0.));
#8489=DIRECTION('ref_axis',(0.,0.,-1.));
#8490=DIRECTION('center_axis',(0.,-1.,0.));
#8491=DIRECTION('ref_axis',(1.,0.,0.));
#8492=DIRECTION('center_axis',(0.,1.,0.));
#8493=DIRECTION('ref_axis',(1.,0.,0.));
#8494=DIRECTION('center_axis',(0.,1.,0.));
#8495=DIRECTION('ref_axis',(1.,0.,0.));
#8496=DIRECTION('',(-0.447213595499958,0.894427190999916,-5.47678698264203E-17));
#8497=DIRECTION('center_axis',(0.,-1.,0.));
#8498=DIRECTION('ref_axis',(1.,0.,0.));
#8499=DIRECTION('center_axis',(0.,1.,0.));
#8500=DIRECTION('ref_axis',(1.,0.,0.));
#8501=DIRECTION('',(0.,1.,0.));
#8502=DIRECTION('center_axis',(0.,1.,0.));
#8503=DIRECTION('ref_axis',(1.,0.,0.));
#8504=DIRECTION('center_axis',(0.,-1.,0.));
#8505=DIRECTION('ref_axis',(1.,0.,0.));
#8506=DIRECTION('',(-0.707106781186547,0.707106781186548,-8.65956056235493E-17));
#8507=DIRECTION('center_axis',(0.,-1.,0.));
#8508=DIRECTION('ref_axis',(0.,0.,-1.));
#8509=DIRECTION('center_axis',(0.866025403784439,0.,-0.5));
#8510=DIRECTION('ref_axis',(0.5,0.,0.866025403784439));
#8511=DIRECTION('',(-0.5,0.,-0.866025403784439));
#8512=DIRECTION('',(0.,-1.,0.));
#8513=DIRECTION('',(0.5,0.,0.866025403784439));
#8514=DIRECTION('',(0.,-1.,0.));
#8515=DIRECTION('center_axis',(1.20185167898973E-16,0.,-1.));
#8516=DIRECTION('ref_axis',(1.,0.,1.20185167898973E-16));
#8517=DIRECTION('',(-1.,0.,-1.20185167898973E-16));
#8518=DIRECTION('',(0.,-1.,0.));
#8519=DIRECTION('',(1.,0.,1.20185167898973E-16));
#8520=DIRECTION('center_axis',(-0.866025403784439,0.,-0.5));
#8521=DIRECTION('ref_axis',(0.5,0.,-0.866025403784439));
#8522=DIRECTION('',(-0.5,0.,0.866025403784439));
#8523=DIRECTION('',(0.,-1.,0.));
#8524=DIRECTION('',(0.5,0.,-0.866025403784439));
#8525=DIRECTION('center_axis',(-0.866025403784439,0.,0.5));
#8526=DIRECTION('ref_axis',(-0.5,0.,-0.866025403784439));
#8527=DIRECTION('',(0.5,0.,0.866025403784439));
#8528=DIRECTION('',(0.,-1.,0.));
#8529=DIRECTION('',(-0.5,0.,-0.866025403784439));
#8530=DIRECTION('center_axis',(-2.40370335797945E-16,0.,1.));
#8531=DIRECTION('ref_axis',(-1.,0.,-2.40370335797945E-16));
#8532=DIRECTION('',(1.,0.,2.40370335797945E-16));
#8533=DIRECTION('',(0.,-1.,0.));
#8534=DIRECTION('',(-1.,0.,-2.40370335797945E-16));
#8535=DIRECTION('center_axis',(0.866025403784439,0.,0.5));
#8536=DIRECTION('ref_axis',(-0.5,0.,0.866025403784439));
#8537=DIRECTION('',(0.5,0.,-0.866025403784439));
#8538=DIRECTION('',(-0.5,0.,0.866025403784439));
#8539=DIRECTION('center_axis',(0.,1.,0.));
#8540=DIRECTION('ref_axis',(1.,0.,0.));
#8541=DIRECTION('center_axis',(0.,-1.,0.));
#8542=DIRECTION('ref_axis',(0.,0.,-1.));
#8543=DIRECTION('axis',(0.,0.,1.));
#8544=DIRECTION('refdir',(1.,0.,0.));
#8545=DIRECTION('axis',(0.,0.,1.));
#8546=DIRECTION('refdir',(1.,0.,0.));
#8547=DIRECTION('center_axis',(0.,1.,0.));
#8548=DIRECTION('ref_axis',(0.,0.,1.));
#8549=DIRECTION('center_axis',(0.,-1.,0.));
#8550=DIRECTION('ref_axis',(1.,0.,0.));
#8551=DIRECTION('',(-1.,0.,0.));
#8552=DIRECTION('',(0.,0.,-1.));
#8553=DIRECTION('',(1.,0.,0.));
#8554=DIRECTION('center_axis',(0.,0.,1.));
#8555=DIRECTION('ref_axis',(1.,0.,0.));
#8556=DIRECTION('',(0.,-1.,0.));
#8557=DIRECTION('',(0.,1.,0.));
#8558=DIRECTION('',(-1.,0.,0.));
#8559=DIRECTION('center_axis',(0.,-1.,0.));
#8560=DIRECTION('ref_axis',(0.,0.,-1.));
#8561=DIRECTION('center_axis',(0.,1.,0.));
#8562=DIRECTION('ref_axis',(1.,0.,0.));
#8563=DIRECTION('',(0.,0.,1.));
#8564=DIRECTION('',(1.,0.,0.));
#8565=DIRECTION('center_axis',(0.,0.,-1.));
#8566=DIRECTION('ref_axis',(-1.,0.,0.));
#8567=DIRECTION('',(0.,1.,0.));
#8568=DIRECTION('',(0.,1.,0.));
#8569=DIRECTION('center_axis',(1.,0.,0.));
#8570=DIRECTION('ref_axis',(0.,0.,-1.));
#8571=DIRECTION('center_axis',(0.,1.,0.));
#8572=DIRECTION('ref_axis',(0.,0.,1.));
#8573=DIRECTION('center_axis',(0.,-1.,0.));
#8574=DIRECTION('ref_axis',(1.,0.,0.));
#8575=DIRECTION('center_axis',(0.,-1.,0.));
#8576=DIRECTION('ref_axis',(1.,0.,0.));
#8577=DIRECTION('center_axis',(0.,-1.,0.));
#8578=DIRECTION('ref_axis',(1.,0.,0.));
#8579=DIRECTION('center_axis',(0.,-1.,0.));
#8580=DIRECTION('ref_axis',(1.,0.,0.));
#8581=DIRECTION('',(0.,1.,0.));
#8582=DIRECTION('center_axis',(0.,-1.,0.));
#8583=DIRECTION('ref_axis',(0.,0.,-1.));
#8584=DIRECTION('center_axis',(0.,-1.,0.));
#8585=DIRECTION('ref_axis',(1.,0.,0.));
#8586=DIRECTION('center_axis',(0.,-1.,0.));
#8587=DIRECTION('ref_axis',(1.,0.,0.));
#8588=DIRECTION('center_axis',(0.,-1.,0.));
#8589=DIRECTION('ref_axis',(1.,0.,0.));
#8590=DIRECTION('',(0.,1.,0.));
#8591=DIRECTION('center_axis',(0.,1.,0.));
#8592=DIRECTION('ref_axis',(0.,0.,1.));
#8593=DIRECTION('center_axis',(0.,-1.,0.));
#8594=DIRECTION('ref_axis',(1.,0.,0.));
#8595=DIRECTION('center_axis',(0.,-1.,0.));
#8596=DIRECTION('ref_axis',(1.,0.,0.));
#8597=DIRECTION('center_axis',(0.,-1.,0.));
#8598=DIRECTION('ref_axis',(1.,0.,0.));
#8599=DIRECTION('',(0.,1.,0.));
#8600=DIRECTION('center_axis',(0.,-1.,0.));
#8601=DIRECTION('ref_axis',(0.,0.,-1.));
#8602=DIRECTION('center_axis',(0.,-1.,0.));
#8603=DIRECTION('ref_axis',(1.,0.,0.));
#8604=DIRECTION('center_axis',(0.,-1.,0.));
#8605=DIRECTION('ref_axis',(1.,0.,0.));
#8606=DIRECTION('center_axis',(0.,-1.,0.));
#8607=DIRECTION('ref_axis',(1.,0.,0.));
#8608=DIRECTION('',(0.,1.,0.));
#8609=DIRECTION('center_axis',(0.,1.,0.));
#8610=DIRECTION('ref_axis',(0.,0.,1.));
#8611=DIRECTION('center_axis',(0.,-1.,0.));
#8612=DIRECTION('ref_axis',(1.,0.,0.));
#8613=DIRECTION('center_axis',(0.,-1.,0.));
#8614=DIRECTION('ref_axis',(1.,0.,0.));
#8615=DIRECTION('center_axis',(0.,-1.,0.));
#8616=DIRECTION('ref_axis',(1.,0.,0.));
#8617=DIRECTION('',(0.,1.,0.));
#8618=DIRECTION('center_axis',(0.,-1.,0.));
#8619=DIRECTION('ref_axis',(0.,0.,-1.));
#8620=DIRECTION('center_axis',(0.,-1.,0.));
#8621=DIRECTION('ref_axis',(1.,0.,0.));
#8622=DIRECTION('center_axis',(0.,-1.,0.));
#8623=DIRECTION('ref_axis',(1.,0.,0.));
#8624=DIRECTION('',(0.,1.,0.));
#8625=DIRECTION('axis',(0.,0.,1.));
#8626=DIRECTION('refdir',(1.,0.,0.));
#8627=DIRECTION('center_axis',(0.,1.,0.));
#8628=DIRECTION('ref_axis',(0.,0.,1.));
#8629=DIRECTION('center_axis',(0.,1.,0.));
#8630=DIRECTION('ref_axis',(1.,0.,0.));
#8631=DIRECTION('',(1.,0.,0.));
#8632=DIRECTION('center_axis',(0.,-1.,0.));
#8633=DIRECTION('ref_axis',(1.,0.,0.));
#8634=DIRECTION('',(-1.,0.,0.));
#8635=DIRECTION('center_axis',(0.,0.,-1.));
#8636=DIRECTION('ref_axis',(-1.,0.,0.));
#8637=DIRECTION('',(0.,-1.,0.));
#8638=DIRECTION('',(0.,1.,0.));
#8639=DIRECTION('',(1.,0.,0.));
#8640=DIRECTION('center_axis',(0.,-1.,0.));
#8641=DIRECTION('ref_axis',(0.,0.,-1.));
#8642=DIRECTION('center_axis',(0.,-1.,0.));
#8643=DIRECTION('ref_axis',(1.,0.,0.));
#8644=DIRECTION('center_axis',(0.,1.,0.));
#8645=DIRECTION('ref_axis',(1.,0.,0.));
#8646=DIRECTION('',(-1.,0.,0.));
#8647=DIRECTION('center_axis',(0.,0.,1.));
#8648=DIRECTION('ref_axis',(1.,0.,0.));
#8649=DIRECTION('',(0.,1.,0.));
#8650=DIRECTION('',(0.,-1.,0.));
#8651=DIRECTION('center_axis',(0.,1.,0.));
#8652=DIRECTION('ref_axis',(0.,0.,1.));
#8653=DIRECTION('center_axis',(0.,-1.,0.));
#8654=DIRECTION('ref_axis',(1.,0.,0.));
#8655=DIRECTION('center_axis',(0.,-1.,0.));
#8656=DIRECTION('ref_axis',(1.,0.,0.));
#8657=DIRECTION('center_axis',(0.,-1.,0.));
#8658=DIRECTION('ref_axis',(1.,0.,0.));
#8659=DIRECTION('center_axis',(0.,-1.,0.));
#8660=DIRECTION('ref_axis',(1.,0.,0.));
#8661=DIRECTION('',(0.,1.,0.));
#8662=DIRECTION('center_axis',(0.,-1.,0.));
#8663=DIRECTION('ref_axis',(0.,0.,-1.));
#8664=DIRECTION('center_axis',(0.,-1.,0.));
#8665=DIRECTION('ref_axis',(1.,0.,0.));
#8666=DIRECTION('center_axis',(0.,-1.,0.));
#8667=DIRECTION('ref_axis',(1.,0.,0.));
#8668=DIRECTION('',(0.,1.,0.));
#8669=DIRECTION('',(0.,0.,1.));
#8670=DIRECTION('',(1.,0.,0.));
#8671=DIRECTION('',(0.,0.,1.));
#8672=DIRECTION('',(1.,0.,0.));
#8673=DIRECTION('axis',(0.,0.,1.));
#8674=DIRECTION('refdir',(1.,0.,0.));
#8675=DIRECTION('center_axis',(0.866025403784439,0.,-0.5));
#8676=DIRECTION('ref_axis',(0.5,0.,0.866025403784439));
#8677=DIRECTION('',(-0.5,0.,-0.866025403784439));
#8678=DIRECTION('',(0.,-1.,0.));
#8679=DIRECTION('',(0.5,0.,0.866025403784439));
#8680=DIRECTION('',(0.,-1.,0.));
#8681=DIRECTION('center_axis',(1.60246890531964E-16,0.,-1.));
#8682=DIRECTION('ref_axis',(1.,0.,1.60246890531964E-16));
#8683=DIRECTION('',(-1.,0.,-1.60246890531964E-16));
#8684=DIRECTION('',(0.,-1.,0.));
#8685=DIRECTION('',(1.,0.,1.60246890531964E-16));
#8686=DIRECTION('center_axis',(-0.866025403784439,0.,-0.5));
#8687=DIRECTION('ref_axis',(0.5,0.,-0.866025403784439));
#8688=DIRECTION('',(-0.5,0.,0.866025403784439));
#8689=DIRECTION('',(0.,-1.,0.));
#8690=DIRECTION('',(0.5,0.,-0.866025403784439));
#8691=DIRECTION('center_axis',(-0.866025403784439,0.,0.5));
#8692=DIRECTION('ref_axis',(-0.5,0.,-0.866025403784439));
#8693=DIRECTION('',(0.5,0.,0.866025403784439));
#8694=DIRECTION('',(0.,-1.,0.));
#8695=DIRECTION('',(-0.5,0.,-0.866025403784439));
#8696=DIRECTION('center_axis',(-1.60246890531964E-16,0.,1.));
#8697=DIRECTION('ref_axis',(-1.,0.,-1.60246890531964E-16));
#8698=DIRECTION('',(1.,0.,1.60246890531964E-16));
#8699=DIRECTION('',(0.,-1.,0.));
#8700=DIRECTION('',(-1.,0.,-1.60246890531964E-16));
#8701=DIRECTION('center_axis',(0.866025403784439,0.,0.5));
#8702=DIRECTION('ref_axis',(-0.5,0.,0.866025403784439));
#8703=DIRECTION('',(0.5,0.,-0.866025403784439));
#8704=DIRECTION('',(-0.5,0.,0.866025403784439));
#8705=DIRECTION('center_axis',(0.,1.,0.));
#8706=DIRECTION('ref_axis',(1.,0.,0.));
#8707=DIRECTION('center_axis',(0.,-1.,0.));
#8708=DIRECTION('ref_axis',(0.,0.,-1.));
#8709=DIRECTION('center_axis',(0.,1.,0.));
#8710=DIRECTION('ref_axis',(1.,0.,0.));
#8711=DIRECTION('center_axis',(0.,1.,0.));
#8712=DIRECTION('ref_axis',(1.,0.,0.));
#8713=DIRECTION('center_axis',(0.,1.,0.));
#8714=DIRECTION('ref_axis',(0.,0.,1.));
#8715=DIRECTION('center_axis',(0.,-1.,0.));
#8716=DIRECTION('ref_axis',(1.,0.,0.));
#8717=DIRECTION('center_axis',(0.,-1.,0.));
#8718=DIRECTION('ref_axis',(1.,0.,0.));
#8719=DIRECTION('center_axis',(0.,-1.,0.));
#8720=DIRECTION('ref_axis',(1.,0.,0.));
#8721=DIRECTION('',(0.707106781186547,0.707106781186548,8.65956056235493E-17));
#8722=DIRECTION('center_axis',(0.,-1.,0.));
#8723=DIRECTION('ref_axis',(1.,0.,0.));
#8724=DIRECTION('center_axis',(0.,-1.,0.));
#8725=DIRECTION('ref_axis',(1.,0.,0.));
#8726=DIRECTION('',(0.,1.,0.));
#8727=DIRECTION('center_axis',(0.,1.,0.));
#8728=DIRECTION('ref_axis',(1.,0.,0.));
#8729=DIRECTION('center_axis',(0.,-1.,0.));
#8730=DIRECTION('ref_axis',(1.,0.,0.));
#8731=DIRECTION('',(-0.707106781186547,0.707106781186548,-8.65956056235493E-17));
#8732=DIRECTION('center_axis',(0.,-1.,0.));
#8733=DIRECTION('ref_axis',(0.,0.,-1.));
#8734=DIRECTION('center_axis',(0.,-1.,0.));
#8735=DIRECTION('ref_axis',(1.,0.,0.));
#8736=DIRECTION('center_axis',(0.,1.,0.));
#8737=DIRECTION('ref_axis',(1.,0.,0.));
#8738=DIRECTION('center_axis',(0.,1.,0.));
#8739=DIRECTION('ref_axis',(1.,0.,0.));
#8740=DIRECTION('',(-0.447213595499958,0.894427190999916,-5.47678698264203E-17));
#8741=DIRECTION('center_axis',(0.,-1.,0.));
#8742=DIRECTION('ref_axis',(1.,0.,0.));
#8743=DIRECTION('',(0.,1.,0.));
#8744=DIRECTION('axis',(0.,0.,1.));
#8745=DIRECTION('refdir',(1.,0.,0.));
#8746=DIRECTION('axis',(0.,0.,1.));
#8747=DIRECTION('refdir',(1.,0.,0.));
#8748=DIRECTION('center_axis',(0.,1.,0.));
#8749=DIRECTION('ref_axis',(1.,0.,0.));
#8750=DIRECTION('center_axis',(0.,1.,0.));
#8751=DIRECTION('ref_axis',(1.,0.,0.));
#8752=DIRECTION('',(0.,1.,0.));
#8753=DIRECTION('center_axis',(0.,-1.,0.));
#8754=DIRECTION('ref_axis',(1.,0.,0.));
#8755=DIRECTION('center_axis',(0.,1.,0.));
#8756=DIRECTION('ref_axis',(1.,0.,0.));
#8757=DIRECTION('center_axis',(0.,1.,0.));
#8758=DIRECTION('ref_axis',(1.,0.,0.));
#8759=DIRECTION('center_axis',(0.,1.,0.));
#8760=DIRECTION('ref_axis',(1.,0.,0.));
#8761=DIRECTION('',(0.,1.,0.));
#8762=DIRECTION('center_axis',(0.,1.,0.));
#8763=DIRECTION('ref_axis',(1.,0.,0.));
#8764=DIRECTION('center_axis',(0.,1.,0.));
#8765=DIRECTION('ref_axis',(1.,0.,0.));
#8766=DIRECTION('center_axis',(-1.,0.,0.));
#8767=DIRECTION('ref_axis',(0.,0.,1.));
#8768=DIRECTION('',(0.,-1.,0.));
#8769=DIRECTION('',(0.,0.,1.));
#8770=DIRECTION('',(0.,1.,0.));
#8771=DIRECTION('',(0.,0.,-1.));
#8772=DIRECTION('center_axis',(0.,1.,0.));
#8773=DIRECTION('ref_axis',(1.,0.,0.));
#8774=DIRECTION('center_axis',(0.,-1.,0.));
#8775=DIRECTION('ref_axis',(1.,0.,0.));
#8776=DIRECTION('',(-1.,0.,0.));
#8777=DIRECTION('',(0.,0.,1.));
#8778=DIRECTION('center_axis',(1.,0.,0.));
#8779=DIRECTION('ref_axis',(0.,0.,-1.));
#8780=DIRECTION('',(0.,1.,0.));
#8781=DIRECTION('',(0.,1.,0.));
#8782=DIRECTION('',(0.,0.,-1.));
#8783=DIRECTION('center_axis',(0.,0.,1.));
#8784=DIRECTION('ref_axis',(1.,0.,0.));
#8785=DIRECTION('',(1.,0.,0.));
#8786=DIRECTION('center_axis',(0.,1.,0.));
#8787=DIRECTION('ref_axis',(0.,0.,1.));
#8788=DIRECTION('center_axis',(0.,1.,0.));
#8789=DIRECTION('ref_axis',(1.,0.,0.));
#8790=DIRECTION('center_axis',(-1.,0.,0.));
#8791=DIRECTION('ref_axis',(0.,0.,1.));
#8792=DIRECTION('',(0.,-1.,0.));
#8793=DIRECTION('',(0.,0.,1.));
#8794=DIRECTION('',(0.,1.,0.));
#8795=DIRECTION('',(0.,0.,-1.));
#8796=DIRECTION('center_axis',(0.,1.,0.));
#8797=DIRECTION('ref_axis',(1.,0.,0.));
#8798=DIRECTION('center_axis',(0.,-1.,0.));
#8799=DIRECTION('ref_axis',(1.,0.,0.));
#8800=DIRECTION('',(-1.,0.,0.));
#8801=DIRECTION('',(0.,0.,1.));
#8802=DIRECTION('center_axis',(1.,0.,0.));
#8803=DIRECTION('ref_axis',(0.,0.,-1.));
#8804=DIRECTION('',(0.,1.,0.));
#8805=DIRECTION('',(0.,1.,0.));
#8806=DIRECTION('',(0.,0.,-1.));
#8807=DIRECTION('center_axis',(0.,0.,1.));
#8808=DIRECTION('ref_axis',(1.,0.,0.));
#8809=DIRECTION('',(1.,0.,0.));
#8810=DIRECTION('center_axis',(0.,1.,0.));
#8811=DIRECTION('ref_axis',(0.,0.,1.));
#8812=DIRECTION('center_axis',(0.,1.,0.));
#8813=DIRECTION('ref_axis',(1.,0.,0.));
#8814=DIRECTION('center_axis',(0.,1.,0.));
#8815=DIRECTION('ref_axis',(1.,0.,0.));
#8816=DIRECTION('center_axis',(0.,1.,0.));
#8817=DIRECTION('ref_axis',(1.,0.,0.));
#8818=DIRECTION('',(0.,-1.,0.));
#8819=DIRECTION('center_axis',(0.,1.,0.));
#8820=DIRECTION('ref_axis',(1.,0.,0.));
#8821=DIRECTION('center_axis',(0.,1.,0.));
#8822=DIRECTION('ref_axis',(1.,0.,0.));
#8823=DIRECTION('center_axis',(0.,1.,0.));
#8824=DIRECTION('ref_axis',(1.,0.,0.));
#8825=DIRECTION('axis',(0.,0.,1.));
#8826=DIRECTION('refdir',(1.,0.,0.));
#8827=DIRECTION('center_axis',(0.,1.,0.));
#8828=DIRECTION('ref_axis',(1.,0.,0.));
#8829=DIRECTION('center_axis',(0.,-1.,0.));
#8830=DIRECTION('ref_axis',(1.,0.,0.));
#8831=DIRECTION('',(0.,-1.,0.));
#8832=DIRECTION('center_axis',(0.,-1.,0.));
#8833=DIRECTION('ref_axis',(1.,0.,0.));
#8834=DIRECTION('center_axis',(0.,1.,0.));
#8835=DIRECTION('ref_axis',(1.,0.,0.));
#8836=DIRECTION('center_axis',(0.,1.,0.));
#8837=DIRECTION('ref_axis',(1.,0.,0.));
#8838=DIRECTION('',(0.,-1.,0.));
#8839=DIRECTION('center_axis',(0.,1.,0.));
#8840=DIRECTION('ref_axis',(1.,0.,0.));
#8841=DIRECTION('center_axis',(0.,1.,0.));
#8842=DIRECTION('ref_axis',(1.,0.,0.));
#8843=DIRECTION('center_axis',(0.,1.,0.));
#8844=DIRECTION('ref_axis',(1.,0.,0.));
#8845=DIRECTION('axis',(0.,0.,1.));
#8846=DIRECTION('refdir',(1.,0.,0.));
#8847=DIRECTION('center_axis',(0.,1.,0.));
#8848=DIRECTION('ref_axis',(1.,0.,0.));
#8849=DIRECTION('center_axis',(0.,-1.,0.));
#8850=DIRECTION('ref_axis',(1.,0.,0.));
#8851=DIRECTION('',(0.,-1.,0.));
#8852=DIRECTION('center_axis',(0.,-1.,0.));
#8853=DIRECTION('ref_axis',(1.,0.,0.));
#8854=DIRECTION('center_axis',(0.,1.,0.));
#8855=DIRECTION('ref_axis',(1.,0.,0.));
#8856=DIRECTION('center_axis',(0.,1.,0.));
#8857=DIRECTION('ref_axis',(1.,0.,0.));
#8858=DIRECTION('',(0.,-1.,0.));
#8859=DIRECTION('center_axis',(0.,1.,0.));
#8860=DIRECTION('ref_axis',(1.,0.,0.));
#8861=DIRECTION('center_axis',(0.,1.,0.));
#8862=DIRECTION('ref_axis',(1.,0.,0.));
#8863=DIRECTION('center_axis',(0.,1.,0.));
#8864=DIRECTION('ref_axis',(1.,0.,0.));
#8865=DIRECTION('axis',(0.,0.,1.));
#8866=DIRECTION('refdir',(1.,0.,0.));
#8867=DIRECTION('center_axis',(0.,1.,0.));
#8868=DIRECTION('ref_axis',(1.,0.,0.));
#8869=DIRECTION('center_axis',(0.,-1.,0.));
#8870=DIRECTION('ref_axis',(1.,0.,0.));
#8871=DIRECTION('',(0.,-1.,0.));
#8872=DIRECTION('center_axis',(0.,-1.,0.));
#8873=DIRECTION('ref_axis',(1.,0.,0.));
#8874=DIRECTION('center_axis',(0.,1.,0.));
#8875=DIRECTION('ref_axis',(1.,0.,0.));
#8876=DIRECTION('center_axis',(0.,1.,0.));
#8877=DIRECTION('ref_axis',(1.,0.,0.));
#8878=DIRECTION('',(0.,-1.,0.));
#8879=DIRECTION('center_axis',(0.,1.,0.));
#8880=DIRECTION('ref_axis',(1.,0.,0.));
#8881=DIRECTION('center_axis',(0.,1.,0.));
#8882=DIRECTION('ref_axis',(1.,0.,0.));
#8883=DIRECTION('center_axis',(0.,1.,0.));
#8884=DIRECTION('ref_axis',(1.,0.,0.));
#8885=DIRECTION('axis',(0.,0.,1.));
#8886=DIRECTION('refdir',(1.,0.,0.));
#8887=DIRECTION('center_axis',(0.,1.,0.));
#8888=DIRECTION('ref_axis',(1.,0.,0.));
#8889=DIRECTION('center_axis',(0.,-1.,0.));
#8890=DIRECTION('ref_axis',(1.,0.,0.));
#8891=DIRECTION('',(0.,-1.,0.));
#8892=DIRECTION('center_axis',(0.,-1.,0.));
#8893=DIRECTION('ref_axis',(1.,0.,0.));
#8894=DIRECTION('center_axis',(0.,1.,0.));
#8895=DIRECTION('ref_axis',(1.,0.,0.));
#8896=DIRECTION('center_axis',(0.,1.,0.));
#8897=DIRECTION('ref_axis',(1.,0.,0.));
#8898=DIRECTION('',(0.,-1.,0.));
#8899=DIRECTION('center_axis',(0.,1.,0.));
#8900=DIRECTION('ref_axis',(1.,0.,0.));
#8901=DIRECTION('center_axis',(0.,1.,0.));
#8902=DIRECTION('ref_axis',(1.,0.,0.));
#8903=DIRECTION('center_axis',(0.,1.,0.));
#8904=DIRECTION('ref_axis',(1.,0.,0.));
#8905=DIRECTION('axis',(0.,0.,1.));
#8906=DIRECTION('refdir',(1.,0.,0.));
#8907=DIRECTION('center_axis',(-1.,0.,0.));
#8908=DIRECTION('ref_axis',(0.,0.,1.));
#8909=DIRECTION('',(0.,0.,1.));
#8910=DIRECTION('',(0.,1.,0.));
#8911=DIRECTION('',(0.,0.,-1.));
#8912=DIRECTION('',(0.,1.,0.));
#8913=DIRECTION('center_axis',(0.,0.,-1.));
#8914=DIRECTION('ref_axis',(-1.,0.,0.));
#8915=DIRECTION('',(-1.,0.,0.));
#8916=DIRECTION('',(0.,1.,0.));
#8917=DIRECTION('',(1.,0.,0.));
#8918=DIRECTION('center_axis',(1.,0.,0.));
#8919=DIRECTION('ref_axis',(0.,0.,-1.));
#8920=DIRECTION('',(0.,0.,-1.));
#8921=DIRECTION('',(0.,-1.,0.));
#8922=DIRECTION('',(0.,0.,1.));
#8923=DIRECTION('center_axis',(0.,1.,0.));
#8924=DIRECTION('ref_axis',(1.,0.,0.));
#8925=DIRECTION('center_axis',(0.,1.,0.));
#8926=DIRECTION('ref_axis',(1.,0.,0.));
#8927=DIRECTION('center_axis',(0.,-1.,0.));
#8928=DIRECTION('ref_axis',(1.,0.,0.));
#8929=DIRECTION('center_axis',(0.,1.,0.));
#8930=DIRECTION('ref_axis',(-1.83697019872103E-16,0.,1.));
#8931=DIRECTION('center_axis',(0.,1.,0.));
#8932=DIRECTION('ref_axis',(1.,0.,0.));
#8933=DIRECTION('center_axis',(0.,1.,0.));
#8934=DIRECTION('ref_axis',(1.,0.,0.));
#8935=DIRECTION('center_axis',(0.,1.,0.));
#8936=DIRECTION('ref_axis',(1.,0.,0.));
#8937=DIRECTION('',(0.,-1.,0.));
#8938=DIRECTION('center_axis',(0.,1.,0.));
#8939=DIRECTION('ref_axis',(1.,0.,0.));
#8940=DIRECTION('center_axis',(0.,1.,0.));
#8941=DIRECTION('ref_axis',(1.,0.,0.));
#8942=DIRECTION('',(0.,-1.,0.));
#8943=DIRECTION('center_axis',(0.,-1.,0.));
#8944=DIRECTION('ref_axis',(1.,0.,0.));
#8945=DIRECTION('center_axis',(0.,1.,0.));
#8946=DIRECTION('ref_axis',(1.,0.,0.));
#8947=DIRECTION('center_axis',(0.,1.,0.));
#8948=DIRECTION('ref_axis',(1.,0.,0.));
#8949=DIRECTION('center_axis',(0.,1.,0.));
#8950=DIRECTION('ref_axis',(1.,0.,0.));
#8951=DIRECTION('',(0.,-1.,0.));
#8952=DIRECTION('center_axis',(0.,1.,0.));
#8953=DIRECTION('ref_axis',(1.,0.,0.));
#8954=DIRECTION('center_axis',(0.,1.,0.));
#8955=DIRECTION('ref_axis',(1.,0.,0.));
#8956=DIRECTION('center_axis',(0.,1.,0.));
#8957=DIRECTION('ref_axis',(1.,0.,0.));
#8958=DIRECTION('axis',(0.,0.,1.));
#8959=DIRECTION('refdir',(1.,0.,0.));
#8960=DIRECTION('center_axis',(0.,1.,0.));
#8961=DIRECTION('ref_axis',(1.,0.,0.));
#8962=DIRECTION('center_axis',(0.,1.,0.));
#8963=DIRECTION('ref_axis',(1.,0.,0.));
#8964=DIRECTION('',(0.,1.,0.));
#8965=DIRECTION('center_axis',(0.,-1.,0.));
#8966=DIRECTION('ref_axis',(1.,0.,0.));
#8967=DIRECTION('center_axis',(-1.,0.,0.));
#8968=DIRECTION('ref_axis',(0.,0.,1.));
#8969=DIRECTION('',(0.,0.,1.));
#8970=DIRECTION('',(0.,1.,0.));
#8971=DIRECTION('',(0.,0.,-1.));
#8972=DIRECTION('',(0.,1.,0.));
#8973=DIRECTION('center_axis',(0.,0.,-1.));
#8974=DIRECTION('ref_axis',(-1.,0.,0.));
#8975=DIRECTION('',(-1.,0.,0.));
#8976=DIRECTION('',(0.,1.,0.));
#8977=DIRECTION('',(1.,0.,0.));
#8978=DIRECTION('center_axis',(1.,0.,0.));
#8979=DIRECTION('ref_axis',(0.,0.,-1.));
#8980=DIRECTION('',(0.,0.,-1.));
#8981=DIRECTION('',(0.,-1.,0.));
#8982=DIRECTION('',(0.,0.,1.));
#8983=DIRECTION('center_axis',(0.,1.,0.));
#8984=DIRECTION('ref_axis',(1.,0.,0.));
#8985=DIRECTION('center_axis',(0.,1.,0.));
#8986=DIRECTION('ref_axis',(1.,0.,0.));
#8987=DIRECTION('center_axis',(0.,-1.,0.));
#8988=DIRECTION('ref_axis',(1.,0.,0.));
#8989=DIRECTION('center_axis',(0.,1.,0.));
#8990=DIRECTION('ref_axis',(-1.83697019872103E-16,0.,1.));
#8991=DIRECTION('center_axis',(0.,-1.,0.));
#8992=DIRECTION('ref_axis',(1.,0.,0.));
#8993=DIRECTION('center_axis',(0.,1.,0.));
#8994=DIRECTION('ref_axis',(1.,0.,0.));
#8995=DIRECTION('',(0.,-1.,0.));
#8996=DIRECTION('center_axis',(0.,1.,0.));
#8997=DIRECTION('ref_axis',(1.,0.,0.));
#8998=DIRECTION('',(0.,1.,0.));
#8999=DIRECTION('center_axis',(0.,1.,0.));
#9000=DIRECTION('ref_axis',(1.,0.,0.));
#9001=DIRECTION('center_axis',(0.,1.,0.));
#9002=DIRECTION('ref_axis',(1.,0.,0.));
#9003=DIRECTION('',(-1.,0.,0.));
#9004=DIRECTION('center_axis',(0.,-1.,0.));
#9005=DIRECTION('ref_axis',(1.,0.,0.));
#9006=DIRECTION('',(1.,0.,0.));
#9007=DIRECTION('center_axis',(0.,0.,1.));
#9008=DIRECTION('ref_axis',(1.,0.,0.));
#9009=DIRECTION('',(1.,0.,0.));
#9010=DIRECTION('',(0.,1.,0.));
#9011=DIRECTION('center_axis',(0.,0.,-1.));
#9012=DIRECTION('ref_axis',(-1.,0.,0.));
#9013=DIRECTION('',(0.,-1.,0.));
#9014=DIRECTION('',(-1.,0.,0.));
#9015=DIRECTION('center_axis',(0.,1.,0.));
#9016=DIRECTION('ref_axis',(0.,0.,1.));
#9017=DIRECTION('center_axis',(0.,1.,0.));
#9018=DIRECTION('ref_axis',(1.,0.,0.));
#9019=DIRECTION('center_axis',(0.,1.,0.));
#9020=DIRECTION('ref_axis',(1.,0.,0.));
#9021=DIRECTION('',(0.,-1.,0.));
#9022=DIRECTION('center_axis',(0.,1.,0.));
#9023=DIRECTION('ref_axis',(1.,0.,0.));
#9024=DIRECTION('center_axis',(0.,1.,0.));
#9025=DIRECTION('ref_axis',(1.,0.,0.));
#9026=DIRECTION('axis',(0.,0.,1.));
#9027=DIRECTION('refdir',(1.,0.,0.));
#9028=DIRECTION('center_axis',(0.,1.,0.));
#9029=DIRECTION('ref_axis',(1.,0.,0.));
#9030=DIRECTION('center_axis',(0.,1.,0.));
#9031=DIRECTION('ref_axis',(1.,0.,0.));
#9032=DIRECTION('',(0.,1.,0.));
#9033=DIRECTION('center_axis',(0.,1.,0.));
#9034=DIRECTION('ref_axis',(1.,0.,0.));
#9035=DIRECTION('center_axis',(0.,1.,0.));
#9036=DIRECTION('ref_axis',(1.,0.,0.));
#9037=DIRECTION('center_axis',(0.,1.,0.));
#9038=DIRECTION('ref_axis',(1.,0.,0.));
#9039=DIRECTION('center_axis',(0.,1.,0.));
#9040=DIRECTION('ref_axis',(1.,0.,0.));
#9041=DIRECTION('',(0.,-1.,0.));
#9042=DIRECTION('center_axis',(0.,1.,0.));
#9043=DIRECTION('ref_axis',(1.,0.,0.));
#9044=DIRECTION('center_axis',(0.,1.,0.));
#9045=DIRECTION('ref_axis',(1.,0.,0.));
#9046=DIRECTION('center_axis',(0.,1.,0.));
#9047=DIRECTION('ref_axis',(1.,0.,0.));
#9048=DIRECTION('axis',(0.,0.,1.));
#9049=DIRECTION('refdir',(1.,0.,0.));
#9050=DIRECTION('center_axis',(0.,1.,0.));
#9051=DIRECTION('ref_axis',(1.,0.,0.));
#9052=DIRECTION('center_axis',(0.,-1.,0.));
#9053=DIRECTION('ref_axis',(1.,0.,0.));
#9054=DIRECTION('',(0.,-1.,0.));
#9055=DIRECTION('center_axis',(0.,-1.,0.));
#9056=DIRECTION('ref_axis',(1.,0.,0.));
#9057=DIRECTION('center_axis',(0.,1.,0.));
#9058=DIRECTION('ref_axis',(1.,0.,0.));
#9059=DIRECTION('center_axis',(0.,1.,0.));
#9060=DIRECTION('ref_axis',(1.,0.,0.));
#9061=DIRECTION('',(0.,-1.,0.));
#9062=DIRECTION('center_axis',(0.,1.,0.));
#9063=DIRECTION('ref_axis',(1.,0.,0.));
#9064=DIRECTION('center_axis',(0.,1.,0.));
#9065=DIRECTION('ref_axis',(1.,0.,0.));
#9066=DIRECTION('center_axis',(0.,1.,0.));
#9067=DIRECTION('ref_axis',(1.,0.,0.));
#9068=DIRECTION('axis',(0.,0.,1.));
#9069=DIRECTION('refdir',(1.,0.,0.));
#9070=DIRECTION('center_axis',(0.,1.,0.));
#9071=DIRECTION('ref_axis',(1.,0.,0.));
#9072=DIRECTION('center_axis',(0.,-1.,0.));
#9073=DIRECTION('ref_axis',(1.,0.,0.));
#9074=DIRECTION('',(0.,-1.,0.));
#9075=DIRECTION('center_axis',(0.,-1.,0.));
#9076=DIRECTION('ref_axis',(1.,0.,0.));
#9077=DIRECTION('center_axis',(0.,1.,0.));
#9078=DIRECTION('ref_axis',(1.,0.,0.));
#9079=DIRECTION('center_axis',(0.,1.,0.));
#9080=DIRECTION('ref_axis',(1.,0.,0.));
#9081=DIRECTION('',(0.,-1.,0.));
#9082=DIRECTION('center_axis',(0.,1.,0.));
#9083=DIRECTION('ref_axis',(1.,0.,0.));
#9084=DIRECTION('center_axis',(0.,1.,0.));
#9085=DIRECTION('ref_axis',(1.,0.,0.));
#9086=DIRECTION('center_axis',(0.,1.,0.));
#9087=DIRECTION('ref_axis',(1.,0.,0.));
#9088=DIRECTION('axis',(0.,0.,1.));
#9089=DIRECTION('refdir',(1.,0.,0.));
#9090=DIRECTION('center_axis',(1.,0.,0.));
#9091=DIRECTION('ref_axis',(0.,0.,-1.));
#9092=DIRECTION('',(0.,0.707106781186547,-0.707106781186548));
#9093=DIRECTION('',(0.,1.,0.));
#9094=DIRECTION('',(0.,0.707106781186547,0.707106781186548));
#9095=DIRECTION('',(0.,0.,1.));
#9096=DIRECTION('',(0.,-0.707106781186548,0.707106781186548));
#9097=DIRECTION('',(0.,-1.,0.));
#9098=DIRECTION('',(0.,-0.707106781186548,-0.707106781186548));
#9099=DIRECTION('',(0.,0.,-1.));
#9100=DIRECTION('center_axis',(0.,-0.707106781186548,-0.707106781186548));
#9101=DIRECTION('ref_axis',(-1.,0.,0.));
#9102=DIRECTION('',(-1.,0.,0.));
#9103=DIRECTION('',(0.,0.707106781186548,-0.707106781186548));
#9104=DIRECTION('',(1.,0.,0.));
#9105=DIRECTION('center_axis',(0.,-1.,0.));
#9106=DIRECTION('ref_axis',(1.,0.,0.));
#9107=DIRECTION('',(1.,0.,0.));
#9108=DIRECTION('',(0.,0.,-1.));
#9109=DIRECTION('center_axis',(0.,-0.707106781186548,0.707106781186547));
#9110=DIRECTION('ref_axis',(1.,0.,0.));
#9111=DIRECTION('',(-1.,0.,0.));
#9112=DIRECTION('',(0.,-0.707106781186547,-0.707106781186548));
#9113=DIRECTION('center_axis',(0.,0.,1.));
#9114=DIRECTION('ref_axis',(1.,0.,0.));
#9115=DIRECTION('',(1.,0.,0.));
#9116=DIRECTION('',(0.,-1.,0.));
#9117=DIRECTION('center_axis',(1.,0.,0.));
#9118=DIRECTION('ref_axis',(0.,0.,-1.));
#9119=DIRECTION('',(0.,-0.707106781186547,0.707106781186548));
#9120=DIRECTION('',(0.,0.,1.));
#9121=DIRECTION('',(0.,0.707106781186548,0.707106781186548));
#9122=DIRECTION('',(0.,1.,0.));
#9123=DIRECTION('center_axis',(0.,0.707106781186548,0.707106781186547));
#9124=DIRECTION('ref_axis',(1.,0.,0.));
#9125=DIRECTION('',(-1.,0.,0.));
#9126=DIRECTION('center_axis',(0.,1.,0.));
#9127=DIRECTION('ref_axis',(-1.,0.,0.));
#9128=DIRECTION('',(1.,0.,0.));
#9129=DIRECTION('center_axis',(0.,0.707106781186548,-0.707106781186548));
#9130=DIRECTION('ref_axis',(-1.,0.,0.));
#9131=DIRECTION('',(-1.,0.,0.));
#9132=DIRECTION('center_axis',(0.,0.,1.));
#9133=DIRECTION('ref_axis',(1.,0.,0.));
#9134=DIRECTION('axis',(0.,0.,1.));
#9135=DIRECTION('refdir',(1.,0.,0.));
#9136=DIRECTION('center_axis',(0.,1.,0.));
#9137=DIRECTION('ref_axis',(0.,0.,1.));
#9138=DIRECTION('center_axis',(0.,-1.,0.));
#9139=DIRECTION('ref_axis',(1.,0.,0.));
#9140=DIRECTION('center_axis',(0.,-1.,0.));
#9141=DIRECTION('ref_axis',(1.,0.,0.));
#9142=DIRECTION('center_axis',(0.,-1.,0.));
#9143=DIRECTION('ref_axis',(1.,0.,0.));
#9144=DIRECTION('',(0.707106781186547,0.707106781186548,8.65956056235493E-17));
#9145=DIRECTION('center_axis',(0.,-1.,0.));
#9146=DIRECTION('ref_axis',(1.,0.,0.));
#9147=DIRECTION('center_axis',(0.,-1.,0.));
#9148=DIRECTION('ref_axis',(1.,0.,0.));
#9149=DIRECTION('',(0.,1.,0.));
#9150=DIRECTION('center_axis',(0.,1.,0.));
#9151=DIRECTION('ref_axis',(1.,0.,0.));
#9152=DIRECTION('center_axis',(0.,-1.,0.));
#9153=DIRECTION('ref_axis',(1.,0.,0.));
#9154=DIRECTION('',(-0.707106781186547,0.707106781186548,-8.65956056235493E-17));
#9155=DIRECTION('center_axis',(0.,-1.,0.));
#9156=DIRECTION('ref_axis',(0.,0.,-1.));
#9157=DIRECTION('center_axis',(0.,-1.,0.));
#9158=DIRECTION('ref_axis',(1.,0.,0.));
#9159=DIRECTION('center_axis',(0.,1.,0.));
#9160=DIRECTION('ref_axis',(1.,0.,0.));
#9161=DIRECTION('center_axis',(0.,1.,0.));
#9162=DIRECTION('ref_axis',(1.,0.,0.));
#9163=DIRECTION('',(-0.447213595499958,0.894427190999916,-5.47678698264203E-17));
#9164=DIRECTION('center_axis',(0.,-1.,0.));
#9165=DIRECTION('ref_axis',(1.,0.,0.));
#9166=DIRECTION('center_axis',(0.,1.,0.));
#9167=DIRECTION('ref_axis',(1.,0.,0.));
#9168=DIRECTION('',(0.,1.,0.));
#9169=DIRECTION('center_axis',(0.,1.,0.));
#9170=DIRECTION('ref_axis',(1.,0.,0.));
#9171=DIRECTION('center_axis',(0.,-1.,0.));
#9172=DIRECTION('ref_axis',(1.,0.,0.));
#9173=DIRECTION('',(-0.707106781186547,0.707106781186548,-8.65956056235493E-17));
#9174=DIRECTION('center_axis',(0.,-1.,0.));
#9175=DIRECTION('ref_axis',(0.,0.,-1.));
#9176=DIRECTION('center_axis',(0.866025403784439,0.,-0.5));
#9177=DIRECTION('ref_axis',(0.5,0.,0.866025403784439));
#9178=DIRECTION('',(-0.5,0.,-0.866025403784439));
#9179=DIRECTION('',(0.,-1.,0.));
#9180=DIRECTION('',(0.5,0.,0.866025403784439));
#9181=DIRECTION('',(0.,-1.,0.));
#9182=DIRECTION('center_axis',(1.60246890531964E-16,0.,-1.));
#9183=DIRECTION('ref_axis',(1.,0.,1.60246890531964E-16));
#9184=DIRECTION('',(-1.,0.,-1.60246890531964E-16));
#9185=DIRECTION('',(0.,-1.,0.));
#9186=DIRECTION('',(1.,0.,1.60246890531964E-16));
#9187=DIRECTION('center_axis',(-0.866025403784439,0.,-0.5));
#9188=DIRECTION('ref_axis',(0.5,0.,-0.866025403784439));
#9189=DIRECTION('',(-0.5,0.,0.866025403784439));
#9190=DIRECTION('',(0.,-1.,0.));
#9191=DIRECTION('',(0.5,0.,-0.866025403784439));
#9192=DIRECTION('center_axis',(-0.866025403784439,0.,0.5));
#9193=DIRECTION('ref_axis',(-0.5,0.,-0.866025403784439));
#9194=DIRECTION('',(0.5,0.,0.866025403784439));
#9195=DIRECTION('',(0.,-1.,0.));
#9196=DIRECTION('',(-0.5,0.,-0.866025403784439));
#9197=DIRECTION('center_axis',(-1.60246890531964E-16,0.,1.));
#9198=DIRECTION('ref_axis',(-1.,0.,-1.60246890531964E-16));
#9199=DIRECTION('',(1.,0.,1.60246890531964E-16));
#9200=DIRECTION('',(0.,-1.,0.));
#9201=DIRECTION('',(-1.,0.,-1.60246890531964E-16));
#9202=DIRECTION('center_axis',(0.866025403784439,0.,0.5));
#9203=DIRECTION('ref_axis',(-0.5,0.,0.866025403784439));
#9204=DIRECTION('',(0.5,0.,-0.866025403784439));
#9205=DIRECTION('',(-0.5,0.,0.866025403784439));
#9206=DIRECTION('center_axis',(0.,1.,0.));
#9207=DIRECTION('ref_axis',(1.,0.,0.));
#9208=DIRECTION('center_axis',(0.,-1.,0.));
#9209=DIRECTION('ref_axis',(0.,0.,-1.));
#9210=DIRECTION('',(0.,0.,1.));
#9211=DIRECTION('',(1.,0.,0.));
#9212=DIRECTION('',(0.,0.,1.));
#9213=DIRECTION('',(1.,0.,0.));
#9214=DIRECTION('',(0.,0.,1.));
#9215=DIRECTION('',(1.,0.,0.));
#9216=DIRECTION('',(0.,0.,1.));
#9217=DIRECTION('',(1.,0.,0.));
#9218=DIRECTION('',(0.,0.,1.));
#9219=DIRECTION('',(1.,0.,0.));
#9220=DIRECTION('',(0.,0.,1.));
#9221=DIRECTION('',(1.,0.,0.));
#9222=DIRECTION('',(0.,0.,1.));
#9223=DIRECTION('',(1.,0.,0.));
#9224=DIRECTION('',(0.,0.,1.));
#9225=DIRECTION('',(1.,0.,0.));
#9226=DIRECTION('',(0.,0.,1.));
#9227=DIRECTION('',(1.,0.,0.));
#9228=DIRECTION('',(0.,0.,1.));
#9229=DIRECTION('',(1.,0.,0.));
#9230=DIRECTION('',(0.,0.,1.));
#9231=DIRECTION('',(1.,0.,0.));
#9232=DIRECTION('',(0.,0.,1.));
#9233=DIRECTION('',(1.,0.,0.));
#9234=DIRECTION('',(0.,-1.,2.22044604925031E-16));
#9235=DIRECTION('',(1.,0.,0.));
#9236=DIRECTION('',(0.,-1.,2.22044604925031E-16));
#9237=DIRECTION('',(1.,0.,0.));
#9238=DIRECTION('',(0.,0.,1.));
#9239=DIRECTION('',(1.,0.,0.));
#9240=DIRECTION('',(0.,0.,1.));
#9241=DIRECTION('',(-1.,1.22464679914735E-16,0.));
#9242=DIRECTION('',(0.,0.,1.));
#9243=DIRECTION('',(-1.,1.22464679914735E-16,0.));
#9244=DIRECTION('',(0.,0.,1.));
#9245=DIRECTION('',(-1.,1.22464679914735E-16,0.));
#9246=DIRECTION('',(0.,0.,1.));
#9247=DIRECTION('',(-1.,1.22464679914735E-16,0.));
#9248=DIRECTION('',(0.,0.,1.));
#9249=DIRECTION('',(1.,0.,0.));
#9250=DIRECTION('',(0.,0.,1.));
#9251=DIRECTION('',(1.,0.,0.));
#9252=DIRECTION('',(0.,0.,1.));
#9253=DIRECTION('',(1.,0.,0.));
#9254=DIRECTION('',(0.,0.,1.));
#9255=DIRECTION('',(1.,0.,0.));
#9256=DIRECTION('',(0.,-1.,2.22044604925031E-16));
#9257=DIRECTION('',(1.,0.,0.));
#9258=DIRECTION('',(0.,-1.,2.22044604925031E-16));
#9259=DIRECTION('',(1.,0.,0.));
#9260=DIRECTION('',(0.,0.,1.));
#9261=DIRECTION('',(1.,0.,0.));
#9262=DIRECTION('',(0.,0.,1.));
#9263=DIRECTION('',(-1.,1.22464679914735E-16,0.));
#9264=DIRECTION('',(0.,0.,1.));
#9265=DIRECTION('',(-1.,1.22464679914735E-16,0.));
#9266=DIRECTION('',(0.,0.,1.));
#9267=DIRECTION('',(-1.,1.22464679914735E-16,0.));
#9268=DIRECTION('',(0.,0.,1.));
#9269=DIRECTION('',(-1.,1.22464679914735E-16,0.));
#9270=DIRECTION('',(0.,0.,1.));
#9271=DIRECTION('',(1.,0.,0.));
#9272=DIRECTION('',(0.,0.,1.));
#9273=DIRECTION('',(1.,0.,0.));
#9274=DIRECTION('',(0.,0.,1.));
#9275=DIRECTION('',(1.,0.,0.));
#9276=DIRECTION('',(0.,0.,1.));
#9277=DIRECTION('',(1.,0.,0.));
#9278=DIRECTION('',(0.,-1.,2.22044604925031E-16));
#9279=DIRECTION('',(1.,0.,0.));
#9280=DIRECTION('',(0.,-1.,2.22044604925031E-16));
#9281=DIRECTION('',(1.,0.,0.));
#9282=DIRECTION('',(0.,-1.,2.22044604925031E-16));
#9283=DIRECTION('',(1.,0.,0.));
#9284=DIRECTION('',(0.,-1.,2.22044604925031E-16));
#9285=DIRECTION('',(1.,0.,0.));
#9286=DIRECTION('',(0.,-1.,2.22044604925031E-16));
#9287=DIRECTION('',(1.,0.,0.));
#9288=DIRECTION('',(0.,-1.,2.22044604925031E-16));
#9289=DIRECTION('',(1.,0.,0.));
#9290=DIRECTION('',(0.,-1.,2.22044604925031E-16));
#9291=DIRECTION('',(1.,0.,0.));
#9292=DIRECTION('',(0.,0.,1.));
#9293=DIRECTION('',(1.,0.,0.));
#9294=DIRECTION('',(0.,0.,1.));
#9295=DIRECTION('',(1.,0.,0.));
#9296=DIRECTION('',(0.,0.,1.));
#9297=DIRECTION('',(1.,0.,0.));
#9298=DIRECTION('',(0.,0.,1.));
#9299=DIRECTION('',(1.,0.,0.));
#9300=DIRECTION('',(0.,0.,1.));
#9301=DIRECTION('',(1.,0.,0.));
#9302=DIRECTION('',(0.,0.,1.));
#9303=DIRECTION('',(1.,0.,0.));
#9304=DIRECTION('',(0.,0.,1.));
#9305=DIRECTION('',(1.,0.,0.));
#9306=DIRECTION('',(0.,0.,1.));
#9307=DIRECTION('',(1.,0.,0.));
#9308=DIRECTION('',(0.,0.,1.));
#9309=DIRECTION('',(1.,0.,0.));
#9310=DIRECTION('',(0.,0.,1.));
#9311=DIRECTION('',(1.,0.,0.));
#9312=DIRECTION('',(8.65956056235493E-17,-8.65956056235493E-17,-1.));
#9313=DIRECTION('',(2.22044604925031E-16,1.,-8.65956056235494E-17));
#9314=DIRECTION('',(8.65956056235493E-17,-8.65956056235493E-17,-1.));
#9315=DIRECTION('',(2.22044604925031E-16,1.,-8.65956056235494E-17));
#9316=DIRECTION('',(0.,0.,1.));
#9317=DIRECTION('',(-1.,1.22464679914735E-16,0.));
#9318=DIRECTION('',(0.,0.,1.));
#9319=DIRECTION('',(-1.,1.22464679914735E-16,0.));
#9320=DIRECTION('',(0.,0.,1.));
#9321=DIRECTION('',(1.,0.,0.));
#9322=DIRECTION('axis',(0.,0.,1.));
#9323=DIRECTION('refdir',(1.,0.,0.));
#9324=DIRECTION('axis',(0.,0.,1.));
#9325=DIRECTION('refdir',(1.,0.,0.));
#9326=DIRECTION('center_axis',(0.,0.,1.));
#9327=DIRECTION('ref_axis',(1.,0.,0.));
#9328=DIRECTION('center_axis',(0.,0.,1.));
#9329=DIRECTION('ref_axis',(1.,0.,0.));
#9330=DIRECTION('',(0.,0.,1.));
#9331=DIRECTION('center_axis',(0.,0.,-1.));
#9332=DIRECTION('ref_axis',(1.,0.,0.));
#9333=DIRECTION('center_axis',(0.,1.,0.));
#9334=DIRECTION('ref_axis',(-1.,0.,0.));
#9335=DIRECTION('',(-1.,0.,0.));
#9336=DIRECTION('',(0.,0.,1.));
#9337=DIRECTION('',(-1.,0.,0.));
#9338=DIRECTION('',(0.,0.,1.));
#9339=DIRECTION('center_axis',(1.,0.,0.));
#9340=DIRECTION('ref_axis',(0.,1.,0.));
#9341=DIRECTION('',(0.,1.,0.));
#9342=DIRECTION('',(0.,1.,0.));
#9343=DIRECTION('',(0.,0.,1.));
#9344=DIRECTION('center_axis',(0.,-1.,0.));
#9345=DIRECTION('ref_axis',(1.,0.,0.));
#9346=DIRECTION('',(1.,0.,0.));
#9347=DIRECTION('',(1.,0.,0.));
#9348=DIRECTION('',(0.,0.,1.));
#9349=DIRECTION('center_axis',(-1.,0.,0.));
#9350=DIRECTION('ref_axis',(0.,-1.,0.));
#9351=DIRECTION('',(0.,-1.,0.));
#9352=DIRECTION('',(0.,-1.,0.));
#9353=DIRECTION('center_axis',(0.,0.,1.));
#9354=DIRECTION('ref_axis',(1.,0.,0.));
#9355=DIRECTION('center_axis',(0.,0.,1.));
#9356=DIRECTION('ref_axis',(1.,0.,0.));
#9357=DIRECTION('axis',(0.,0.,1.));
#9358=DIRECTION('refdir',(1.,0.,0.));
#9359=DIRECTION('center_axis',(0.,0.,1.));
#9360=DIRECTION('ref_axis',(1.,0.,0.));
#9361=DIRECTION('center_axis',(0.,0.,1.));
#9362=DIRECTION('ref_axis',(1.,0.,0.));
#9363=DIRECTION('center_axis',(0.,0.,1.));
#9364=DIRECTION('ref_axis',(1.,0.,0.));
#9365=DIRECTION('center_axis',(0.,0.,1.));
#9366=DIRECTION('ref_axis',(1.,0.,0.));
#9367=DIRECTION('center_axis',(0.,0.,1.));
#9368=DIRECTION('ref_axis',(1.,0.,0.));
#9369=DIRECTION('',(0.,0.,-1.));
#9370=DIRECTION('center_axis',(0.,0.,1.));
#9371=DIRECTION('ref_axis',(1.,0.,0.));
#9372=DIRECTION('center_axis',(0.,0.,1.));
#9373=DIRECTION('ref_axis',(1.,0.,0.));
#9374=DIRECTION('center_axis',(0.,0.,1.));
#9375=DIRECTION('ref_axis',(1.,0.,0.));
#9376=DIRECTION('',(0.,0.,-1.));
#9377=DIRECTION('center_axis',(0.,0.,1.));
#9378=DIRECTION('ref_axis',(1.,0.,0.));
#9379=DIRECTION('center_axis',(0.,0.,1.));
#9380=DIRECTION('ref_axis',(1.,0.,0.));
#9381=DIRECTION('center_axis',(0.,0.,1.));
#9382=DIRECTION('ref_axis',(1.,0.,0.));
#9383=DIRECTION('',(0.,0.,-1.));
#9384=DIRECTION('center_axis',(0.,0.,1.));
#9385=DIRECTION('ref_axis',(1.,0.,0.));
#9386=DIRECTION('center_axis',(0.,0.,1.));
#9387=DIRECTION('ref_axis',(1.,0.,0.));
#9388=DIRECTION('axis',(0.,0.,1.));
#9389=DIRECTION('refdir',(1.,0.,0.));
#9390=DIRECTION('center_axis',(0.,0.,1.));
#9391=DIRECTION('ref_axis',(1.,0.,0.));
#9392=DIRECTION('center_axis',(0.,0.,-1.));
#9393=DIRECTION('ref_axis',(1.,0.,0.));
#9394=DIRECTION('',(0.,0.,-1.));
#9395=DIRECTION('center_axis',(0.,0.,-1.));
#9396=DIRECTION('ref_axis',(1.,0.,0.));
#9397=DIRECTION('center_axis',(0.,0.,1.));
#9398=DIRECTION('ref_axis',(1.,0.,0.));
#9399=DIRECTION('center_axis',(0.,0.,1.));
#9400=DIRECTION('ref_axis',(1.,0.,0.));
#9401=DIRECTION('',(0.,0.,-1.));
#9402=DIRECTION('center_axis',(0.,0.,1.));
#9403=DIRECTION('ref_axis',(1.,0.,0.));
#9404=DIRECTION('center_axis',(0.,0.,1.));
#9405=DIRECTION('ref_axis',(1.,0.,0.));
#9406=DIRECTION('center_axis',(0.,0.,1.));
#9407=DIRECTION('ref_axis',(1.,0.,0.));
#9408=DIRECTION('',(0.,0.,1.));
#9409=DIRECTION('',(1.,0.,0.));
#9410=DIRECTION('',(0.,0.,1.));
#9411=DIRECTION('',(1.,0.,0.));
#9412=DIRECTION('',(0.,0.,1.));
#9413=DIRECTION('',(1.,0.,0.));
#9414=DIRECTION('',(0.,0.,1.));
#9415=DIRECTION('',(1.,0.,0.));
#9416=DIRECTION('',(0.,0.,1.));
#9417=DIRECTION('',(1.,0.,0.));
#9418=DIRECTION('',(0.,0.,1.));
#9419=DIRECTION('',(1.,0.,0.));
#9420=CARTESIAN_POINT('',(0.,0.,0.));
#9421=CARTESIAN_POINT('',(0.,0.,0.));
#9422=CARTESIAN_POINT('',(0.,0.,0.));
#9423=CARTESIAN_POINT('Origin',(-3.5,4.4,0.6));
#9424=CARTESIAN_POINT('',(3.5,4.4,1.));
#9425=CARTESIAN_POINT('',(-3.5,4.4,1.));
#9426=CARTESIAN_POINT('',(-1.75,4.4,1.));
#9427=CARTESIAN_POINT('',(3.5,4.4,0.6));
#9428=CARTESIAN_POINT('',(3.5,4.4,0.6));
#9429=CARTESIAN_POINT('',(-3.5,4.4,0.6));
#9430=CARTESIAN_POINT('',(-3.5,4.4,0.6));
#9431=CARTESIAN_POINT('',(-3.5,4.4,0.6));
#9432=CARTESIAN_POINT('Origin',(-3.5,8.5,0.6));
#9433=CARTESIAN_POINT('',(-3.5,8.5,1.));
#9434=CARTESIAN_POINT('',(-3.5,5.125,1.));
#9435=CARTESIAN_POINT('',(-3.5,8.5,0.6));
#9436=CARTESIAN_POINT('',(-3.5,8.5,0.6));
#9437=CARTESIAN_POINT('',(-3.5,8.5,0.6));
#9438=CARTESIAN_POINT('Origin',(3.5,8.5,0.6));
#9439=CARTESIAN_POINT('',(3.5,8.5,1.));
#9440=CARTESIAN_POINT('',(1.75,8.5,1.));
#9441=CARTESIAN_POINT('',(3.5,8.5,0.6));
#9442=CARTESIAN_POINT('',(3.5,8.5,0.6));
#9443=CARTESIAN_POINT('',(3.5,8.5,0.6));
#9444=CARTESIAN_POINT('Origin',(3.5,4.4,0.6));
#9445=CARTESIAN_POINT('',(3.5,3.075,1.));
#9446=CARTESIAN_POINT('',(3.5,4.4,0.6));
#9447=CARTESIAN_POINT('Origin',(0.,6.45,0.6));
#9448=CARTESIAN_POINT('Origin',(3.75,0.,-0.1));
#9449=CARTESIAN_POINT('',(3.54,-2.57175827820944E-17,0.));
#9450=CARTESIAN_POINT('Origin',(3.75,0.,0.));
#9451=CARTESIAN_POINT('',(3.54,2.57175827820944E-17,1.));
#9452=CARTESIAN_POINT('',(3.54,-2.57175827820944E-17,-0.1));
#9453=CARTESIAN_POINT('Origin',(3.75,0.,1.));
#9454=CARTESIAN_POINT('Origin',(-3.75,0.,-0.1));
#9455=CARTESIAN_POINT('',(-3.96,-2.57175827820944E-17,0.));
#9456=CARTESIAN_POINT('Origin',(-3.75,0.,0.));
#9457=CARTESIAN_POINT('',(-3.96,2.57175827820944E-17,1.));
#9458=CARTESIAN_POINT('',(-3.96,-2.57175827820944E-17,-0.1));
#9459=CARTESIAN_POINT('Origin',(-3.75,0.,1.));
#9460=CARTESIAN_POINT('Origin',(-3.,2.5,-0.1));
#9461=CARTESIAN_POINT('',(-3.165,2.5,0.));
#9462=CARTESIAN_POINT('Origin',(-3.,2.5,0.));
#9463=CARTESIAN_POINT('',(-3.165,2.5,1.));
#9464=CARTESIAN_POINT('',(-3.165,2.5,-0.1));
#9465=CARTESIAN_POINT('Origin',(-3.,2.5,1.));
#9466=CARTESIAN_POINT('Origin',(3.,2.5,-0.1));
#9467=CARTESIAN_POINT('',(2.835,2.5,0.));
#9468=CARTESIAN_POINT('Origin',(3.,2.5,0.));
#9469=CARTESIAN_POINT('',(2.835,2.5,1.));
#9470=CARTESIAN_POINT('',(2.835,2.5,-0.1));
#9471=CARTESIAN_POINT('Origin',(3.,2.5,1.));
#9472=CARTESIAN_POINT('Origin',(-3.,-2.5,-0.1));
#9473=CARTESIAN_POINT('',(-3.165,-2.5,0.));
#9474=CARTESIAN_POINT('Origin',(-3.,-2.5,0.));
#9475=CARTESIAN_POINT('',(-3.165,-2.5,1.));
#9476=CARTESIAN_POINT('',(-3.165,-2.5,-0.1));
#9477=CARTESIAN_POINT('Origin',(-3.,-2.5,1.));
#9478=CARTESIAN_POINT('Origin',(3.,-2.5,-0.1));
#9479=CARTESIAN_POINT('',(2.835,-2.5,0.));
#9480=CARTESIAN_POINT('Origin',(3.,-2.5,0.));
#9481=CARTESIAN_POINT('',(2.835,-2.5,1.));
#9482=CARTESIAN_POINT('',(2.835,-2.5,-0.1));
#9483=CARTESIAN_POINT('Origin',(3.,-2.5,1.));
#9484=CARTESIAN_POINT('Origin',(6.,9.,0.));
#9485=CARTESIAN_POINT('',(6.,9.,0.));
#9486=CARTESIAN_POINT('',(-6.,9.,0.));
#9487=CARTESIAN_POINT('',(6.,9.,0.));
#9488=CARTESIAN_POINT('',(-6.,9.,1.));
#9489=CARTESIAN_POINT('',(-6.,9.,0.));
#9490=CARTESIAN_POINT('',(6.,9.,1.));
#9491=CARTESIAN_POINT('',(6.,9.,1.));
#9492=CARTESIAN_POINT('',(6.,9.,0.));
#9493=CARTESIAN_POINT('Origin',(6.,-5.5,0.));
#9494=CARTESIAN_POINT('',(6.,-5.5,0.));
#9495=CARTESIAN_POINT('',(6.,-5.5,0.));
#9496=CARTESIAN_POINT('',(6.,-5.5,1.));
#9497=CARTESIAN_POINT('',(6.,-5.5,1.));
#9498=CARTESIAN_POINT('',(6.,-5.5,0.));
#9499=CARTESIAN_POINT('Origin',(-6.,-5.5,0.));
#9500=CARTESIAN_POINT('',(-6.,-5.5,0.));
#9501=CARTESIAN_POINT('',(-6.,-5.5,0.));
#9502=CARTESIAN_POINT('',(-6.,-5.5,1.));
#9503=CARTESIAN_POINT('',(-6.,-5.5,1.));
#9504=CARTESIAN_POINT('',(-6.,-5.5,0.));
#9505=CARTESIAN_POINT('Origin',(-6.,9.,0.));
#9506=CARTESIAN_POINT('',(-6.,9.,0.));
#9507=CARTESIAN_POINT('',(-6.,9.,1.));
#9508=CARTESIAN_POINT('Origin',(0.,1.75,1.));
#9509=CARTESIAN_POINT('Origin',(0.,1.75,0.));
#9510=CARTESIAN_POINT('',(0.,0.,0.));
#9511=CARTESIAN_POINT('Origin',(-5.,9.,-0.8));
#9512=CARTESIAN_POINT('',(-5.,9.,-0.8));
#9513=CARTESIAN_POINT('',(-6.,9.,-0.8));
#9514=CARTESIAN_POINT('',(-5.,9.,-0.8));
#9515=CARTESIAN_POINT('',(-6.,9.,0.));
#9516=CARTESIAN_POINT('',(-6.,9.,-0.8));
#9517=CARTESIAN_POINT('',(-5.,9.,0.));
#9518=CARTESIAN_POINT('',(-5.,9.,0.));
#9519=CARTESIAN_POINT('',(-5.,9.,-0.8));
#9520=CARTESIAN_POINT('Origin',(-5.,-5.5,-0.8));
#9521=CARTESIAN_POINT('',(-5.,-5.5,-0.8));
#9522=CARTESIAN_POINT('',(-5.,-5.5,-0.8));
#9523=CARTESIAN_POINT('',(-5.,-5.5,0.));
#9524=CARTESIAN_POINT('',(-5.,-5.5,0.));
#9525=CARTESIAN_POINT('',(-5.,-5.5,-0.8));
#9526=CARTESIAN_POINT('Origin',(-6.,-5.5,-0.8));
#9527=CARTESIAN_POINT('',(-6.,-5.5,-0.8));
#9528=CARTESIAN_POINT('',(-6.,-5.5,-0.8));
#9529=CARTESIAN_POINT('',(-6.,-5.5,0.));
#9530=CARTESIAN_POINT('',(-6.,-5.5,0.));
#9531=CARTESIAN_POINT('',(-6.,-5.5,-0.8));
#9532=CARTESIAN_POINT('Origin',(-6.,9.,-0.8));
#9533=CARTESIAN_POINT('',(-6.,9.,-0.8));
#9534=CARTESIAN_POINT('',(-6.,9.,0.));
#9535=CARTESIAN_POINT('Origin',(-5.5,1.75,0.));
#9536=CARTESIAN_POINT('Origin',(-5.5,1.75,-0.8));
#9537=CARTESIAN_POINT('',(0.,0.,0.));
#9538=CARTESIAN_POINT('Origin',(6.,9.,-0.8));
#9539=CARTESIAN_POINT('',(6.,9.,-0.8));
#9540=CARTESIAN_POINT('',(5.,9.,-0.8));
#9541=CARTESIAN_POINT('',(6.,9.,-0.8));
#9542=CARTESIAN_POINT('',(5.,9.,0.));
#9543=CARTESIAN_POINT('',(5.,9.,-0.8));
#9544=CARTESIAN_POINT('',(6.,9.,0.));
#9545=CARTESIAN_POINT('',(6.,9.,0.));
#9546=CARTESIAN_POINT('',(6.,9.,-0.8));
#9547=CARTESIAN_POINT('Origin',(6.,-5.5,-0.8));
#9548=CARTESIAN_POINT('',(6.,-5.5,-0.8));
#9549=CARTESIAN_POINT('',(6.,-5.5,-0.8));
#9550=CARTESIAN_POINT('',(6.,-5.5,0.));
#9551=CARTESIAN_POINT('',(6.,-5.5,0.));
#9552=CARTESIAN_POINT('',(6.,-5.5,-0.8));
#9553=CARTESIAN_POINT('Origin',(5.,-5.5,-0.8));
#9554=CARTESIAN_POINT('',(5.,-5.5,-0.8));
#9555=CARTESIAN_POINT('',(5.,-5.5,-0.8));
#9556=CARTESIAN_POINT('',(5.,-5.5,0.));
#9557=CARTESIAN_POINT('',(5.,-5.5,0.));
#9558=CARTESIAN_POINT('',(5.,-5.5,-0.8));
#9559=CARTESIAN_POINT('Origin',(5.,9.,-0.8));
#9560=CARTESIAN_POINT('',(5.,9.,-0.8));
#9561=CARTESIAN_POINT('',(5.,9.,0.));
#9562=CARTESIAN_POINT('Origin',(5.5,1.75,0.));
#9563=CARTESIAN_POINT('Origin',(5.5,1.75,-0.8));
#9564=CARTESIAN_POINT('',(0.,0.,0.));
#9565=CARTESIAN_POINT('Origin',(-3.,-2.5,0.9));
#9566=CARTESIAN_POINT('',(-3.225,-2.5,1.));
#9567=CARTESIAN_POINT('Origin',(-3.,-2.5,1.));
#9568=CARTESIAN_POINT('',(-3.225,-2.5,1.8));
#9569=CARTESIAN_POINT('',(-3.225,-2.5,0.9));
#9570=CARTESIAN_POINT('Origin',(-3.,-2.5,1.8));
#9571=CARTESIAN_POINT('Origin',(3.,-2.5,0.9));
#9572=CARTESIAN_POINT('',(2.775,-2.5,1.));
#9573=CARTESIAN_POINT('Origin',(3.,-2.5,1.));
#9574=CARTESIAN_POINT('',(2.775,-2.5,1.8));
#9575=CARTESIAN_POINT('',(2.775,-2.5,0.9));
#9576=CARTESIAN_POINT('Origin',(3.,-2.5,1.8));
#9577=CARTESIAN_POINT('Origin',(-1.4142135623731,-3.4,2.58578643762691));
#9578=CARTESIAN_POINT('',(-1.5792135623731,-3.3,2.58578643762691));
#9579=CARTESIAN_POINT('Origin',(-1.4142135623731,-3.3,2.58578643762691));
#9580=CARTESIAN_POINT('',(-1.5792135623731,-1.7,2.58578643762691));
#9581=CARTESIAN_POINT('',(-1.5792135623731,-3.4,2.58578643762691));
#9582=CARTESIAN_POINT('Origin',(-1.4142135623731,-1.7,2.58578643762691));
#9583=CARTESIAN_POINT('Origin',(-1.41421356237309,-3.4,5.41421356237309));
#9584=CARTESIAN_POINT('',(-1.57921356237309,-3.3,5.41421356237309));
#9585=CARTESIAN_POINT('Origin',(-1.41421356237309,-3.3,5.41421356237309));
#9586=CARTESIAN_POINT('',(-1.57921356237309,-1.7,5.41421356237309));
#9587=CARTESIAN_POINT('',(-1.57921356237309,-3.4,5.41421356237309));
#9588=CARTESIAN_POINT('Origin',(-1.41421356237309,-1.7,5.41421356237309));
#9589=CARTESIAN_POINT('Origin',(1.4142135623731,-3.4,5.41421356237309));
#9590=CARTESIAN_POINT('',(1.2492135623731,-3.3,5.41421356237309));
#9591=CARTESIAN_POINT('Origin',(1.4142135623731,-3.3,5.41421356237309));
#9592=CARTESIAN_POINT('',(1.2492135623731,-1.7,5.41421356237309));
#9593=CARTESIAN_POINT('',(1.2492135623731,-3.4,5.41421356237309));
#9594=CARTESIAN_POINT('Origin',(1.4142135623731,-1.7,5.41421356237309));
#9595=CARTESIAN_POINT('Origin',(1.41421356237309,-3.4,2.5857864376269));
#9596=CARTESIAN_POINT('',(1.24921356237309,-3.3,2.5857864376269));
#9597=CARTESIAN_POINT('Origin',(1.41421356237309,-3.3,2.5857864376269));
#9598=CARTESIAN_POINT('',(1.24921356237309,-1.7,2.5857864376269));
#9599=CARTESIAN_POINT('',(1.24921356237309,-3.4,2.5857864376269));
#9600=CARTESIAN_POINT('Origin',(1.41421356237309,-1.7,2.5857864376269));
#9601=CARTESIAN_POINT('Origin',(0.,-3.4,4.));
#9602=CARTESIAN_POINT('',(-1.6,-3.3,4.));
#9603=CARTESIAN_POINT('Origin',(0.,-3.3,4.));
#9604=CARTESIAN_POINT('',(-1.6,-1.7,4.));
#9605=CARTESIAN_POINT('',(-1.6,-3.4,4.));
#9606=CARTESIAN_POINT('Origin',(0.,-1.7,4.));
#9607=CARTESIAN_POINT('Origin',(-3.6,-3.3,1.8));
#9608=CARTESIAN_POINT('',(2.4,-3.3,1.8));
#9609=CARTESIAN_POINT('',(2.4,-1.7,1.8));
#9610=CARTESIAN_POINT('',(2.4,-3.3,1.8));
#9611=CARTESIAN_POINT('',(3.6,-3.3,1.8));
#9612=CARTESIAN_POINT('',(3.6,-3.3,1.8));
#9613=CARTESIAN_POINT('',(3.6,-1.7,1.8));
#9614=CARTESIAN_POINT('',(3.6,-3.3,1.8));
#9615=CARTESIAN_POINT('',(3.6,-1.7,1.8));
#9616=CARTESIAN_POINT('Origin',(-3.6,-3.3,1.8));
#9617=CARTESIAN_POINT('',(-2.4,-1.7,1.8));
#9618=CARTESIAN_POINT('',(-2.4,-3.3,1.8));
#9619=CARTESIAN_POINT('',(-2.4,-2.5,1.8));
#9620=CARTESIAN_POINT('',(-3.6,-1.7,1.8));
#9621=CARTESIAN_POINT('',(3.6,-1.7,1.8));
#9622=CARTESIAN_POINT('',(-3.6,-3.3,1.8));
#9623=CARTESIAN_POINT('',(-3.6,-3.3,1.8));
#9624=CARTESIAN_POINT('',(3.6,-3.3,1.8));
#9625=CARTESIAN_POINT('Origin',(-3.6,-3.3,1.));
#9626=CARTESIAN_POINT('',(-3.6,-3.3,1.));
#9627=CARTESIAN_POINT('',(-3.6,-3.3,1.8));
#9628=CARTESIAN_POINT('',(-3.6,-1.7,1.));
#9629=CARTESIAN_POINT('',(-3.6,-1.7,1.8));
#9630=CARTESIAN_POINT('',(-3.6,-3.3,1.));
#9631=CARTESIAN_POINT('Origin',(3.6,-3.3,1.8));
#9632=CARTESIAN_POINT('',(3.6,-3.3,1.));
#9633=CARTESIAN_POINT('',(3.6,-3.3,1.));
#9634=CARTESIAN_POINT('',(3.6,-1.7,1.));
#9635=CARTESIAN_POINT('',(3.6,-3.3,1.));
#9636=CARTESIAN_POINT('',(3.6,-1.7,1.));
#9637=CARTESIAN_POINT('Origin',(-2.4,-3.3,1.));
#9638=CARTESIAN_POINT('',(2.4,-3.3,6.5));
#9639=CARTESIAN_POINT('',(2.4,-3.3,1.));
#9640=CARTESIAN_POINT('',(-2.4,-3.3,6.5));
#9641=CARTESIAN_POINT('',(-2.4,-3.3,6.5));
#9642=CARTESIAN_POINT('',(-2.4,-3.3,1.));
#9643=CARTESIAN_POINT('',(-3.6,-3.3,1.));
#9644=CARTESIAN_POINT('Origin',(2.4,-3.3,1.));
#9645=CARTESIAN_POINT('',(2.4,-1.7,6.5));
#9646=CARTESIAN_POINT('',(2.4,-1.7,1.));
#9647=CARTESIAN_POINT('',(2.4,-3.3,6.5));
#9648=CARTESIAN_POINT('Origin',(2.4,-1.7,1.));
#9649=CARTESIAN_POINT('',(-2.4,-1.7,6.5));
#9650=CARTESIAN_POINT('',(-2.4,-1.7,1.));
#9651=CARTESIAN_POINT('',(2.4,-1.7,6.5));
#9652=CARTESIAN_POINT('',(-3.6,-1.7,1.));
#9653=CARTESIAN_POINT('Origin',(-2.4,-1.7,1.));
#9654=CARTESIAN_POINT('',(-2.4,-1.7,6.5));
#9655=CARTESIAN_POINT('Origin',(0.,-2.5,6.5));
#9656=CARTESIAN_POINT('Origin',(0.,-2.5,1.));
#9657=CARTESIAN_POINT('',(0.,0.,0.));
#9658=CARTESIAN_POINT('Origin',(-1.4142135623731,-3.6,2.58578643762691));
#9659=CARTESIAN_POINT('',(-1.6392135623731,-3.5,2.58578643762691));
#9660=CARTESIAN_POINT('Origin',(-1.4142135623731,-3.5,2.58578643762691));
#9661=CARTESIAN_POINT('',(-1.6392135623731,-3.3,2.58578643762691));
#9662=CARTESIAN_POINT('',(-1.6392135623731,-3.6,2.58578643762691));
#9663=CARTESIAN_POINT('Origin',(-1.4142135623731,-3.3,2.58578643762691));
#9664=CARTESIAN_POINT('Origin',(-1.41421356237309,-3.6,5.41421356237309));
#9665=CARTESIAN_POINT('',(-1.6392135623731,-3.5,5.41421356237309));
#9666=CARTESIAN_POINT('Origin',(-1.41421356237309,-3.5,5.41421356237309));
#9667=CARTESIAN_POINT('',(-1.6392135623731,-3.3,5.41421356237309));
#9668=CARTESIAN_POINT('',(-1.6392135623731,-3.6,5.41421356237309));
#9669=CARTESIAN_POINT('Origin',(-1.41421356237309,-3.3,5.41421356237309));
#9670=CARTESIAN_POINT('Origin',(1.4142135623731,-3.6,5.41421356237309));
#9671=CARTESIAN_POINT('',(1.1892135623731,-3.5,5.41421356237309));
#9672=CARTESIAN_POINT('Origin',(1.4142135623731,-3.5,5.41421356237309));
#9673=CARTESIAN_POINT('',(1.1892135623731,-3.3,5.41421356237309));
#9674=CARTESIAN_POINT('',(1.1892135623731,-3.6,5.41421356237309));
#9675=CARTESIAN_POINT('Origin',(1.4142135623731,-3.3,5.41421356237309));
#9676=CARTESIAN_POINT('Origin',(1.41421356237309,-3.6,2.5857864376269));
#9677=CARTESIAN_POINT('',(1.18921356237309,-3.5,2.5857864376269));
#9678=CARTESIAN_POINT('Origin',(1.41421356237309,-3.5,2.5857864376269));
#9679=CARTESIAN_POINT('',(1.18921356237309,-3.3,2.5857864376269));
#9680=CARTESIAN_POINT('',(1.18921356237309,-3.6,2.5857864376269));
#9681=CARTESIAN_POINT('Origin',(1.41421356237309,-3.3,2.5857864376269));
#9682=CARTESIAN_POINT('Origin',(0.,-3.3,4.));
#9683=CARTESIAN_POINT('',(-1.59,-3.,4.));
#9684=CARTESIAN_POINT('Origin',(0.,-3.,4.));
#9685=CARTESIAN_POINT('',(-1.59,-3.3,4.));
#9686=CARTESIAN_POINT('',(-1.59,-3.3,4.));
#9687=CARTESIAN_POINT('Origin',(0.,-3.3,4.));
#9688=CARTESIAN_POINT('Origin',(0.,-3.,4.));
#9689=CARTESIAN_POINT('',(-1.005,-3.,4.));
#9690=CARTESIAN_POINT('Origin',(0.,-3.,4.));
#9691=CARTESIAN_POINT('Origin',(0.,-3.5,4.));
#9692=CARTESIAN_POINT('',(-1.005,-3.5,4.));
#9693=CARTESIAN_POINT('',(-1.005,-3.5,4.));
#9694=CARTESIAN_POINT('Origin',(0.,-3.5,4.));
#9695=CARTESIAN_POINT('Origin',(0.,-3.5,4.));
#9696=CARTESIAN_POINT('',(-2.4,-3.3,4.));
#9697=CARTESIAN_POINT('Origin',(0.,-3.3,4.));
#9698=CARTESIAN_POINT('',(-2.4,-3.5,4.));
#9699=CARTESIAN_POINT('',(-2.4,-3.5,4.));
#9700=CARTESIAN_POINT('Origin',(0.,-3.5,4.));
#9701=CARTESIAN_POINT('Origin',(0.,-3.3,4.));
#9702=CARTESIAN_POINT('Origin',(0.,-3.5,4.));
#9703=CARTESIAN_POINT('',(0.,0.,0.));
#9704=CARTESIAN_POINT('Origin',(-1.4142135623731,-1.8,2.58578643762691));
#9705=CARTESIAN_POINT('',(-1.6392135623731,-1.7,2.58578643762691));
#9706=CARTESIAN_POINT('Origin',(-1.4142135623731,-1.7,2.58578643762691));
#9707=CARTESIAN_POINT('',(-1.6392135623731,-1.5,2.58578643762691));
#9708=CARTESIAN_POINT('',(-1.6392135623731,-1.8,2.58578643762691));
#9709=CARTESIAN_POINT('Origin',(-1.4142135623731,-1.5,2.58578643762691));
#9710=CARTESIAN_POINT('Origin',(-1.41421356237309,-1.8,5.41421356237309));
#9711=CARTESIAN_POINT('',(-1.6392135623731,-1.7,5.41421356237309));
#9712=CARTESIAN_POINT('Origin',(-1.41421356237309,-1.7,5.41421356237309));
#9713=CARTESIAN_POINT('',(-1.6392135623731,-1.5,5.41421356237309));
#9714=CARTESIAN_POINT('',(-1.6392135623731,-1.8,5.41421356237309));
#9715=CARTESIAN_POINT('Origin',(-1.41421356237309,-1.5,5.41421356237309));
#9716=CARTESIAN_POINT('Origin',(1.4142135623731,-1.8,5.41421356237309));
#9717=CARTESIAN_POINT('',(1.1892135623731,-1.7,5.41421356237309));
#9718=CARTESIAN_POINT('Origin',(1.4142135623731,-1.7,5.41421356237309));
#9719=CARTESIAN_POINT('',(1.1892135623731,-1.5,5.41421356237309));
#9720=CARTESIAN_POINT('',(1.1892135623731,-1.8,5.41421356237309));
#9721=CARTESIAN_POINT('Origin',(1.4142135623731,-1.5,5.41421356237309));
#9722=CARTESIAN_POINT('Origin',(1.41421356237309,-1.8,2.5857864376269));
#9723=CARTESIAN_POINT('',(1.18921356237309,-1.7,2.5857864376269));
#9724=CARTESIAN_POINT('Origin',(1.41421356237309,-1.7,2.5857864376269));
#9725=CARTESIAN_POINT('',(1.18921356237309,-1.5,2.5857864376269));
#9726=CARTESIAN_POINT('',(1.18921356237309,-1.8,2.5857864376269));
#9727=CARTESIAN_POINT('Origin',(1.41421356237309,-1.5,2.5857864376269));
#9728=CARTESIAN_POINT('Origin',(0.,-2.,4.));
#9729=CARTESIAN_POINT('',(-1.59,-1.7,4.));
#9730=CARTESIAN_POINT('Origin',(0.,-1.7,4.));
#9731=CARTESIAN_POINT('',(-1.59,-2.,4.));
#9732=CARTESIAN_POINT('',(-1.59,-2.,4.));
#9733=CARTESIAN_POINT('Origin',(0.,-2.,4.));
#9734=CARTESIAN_POINT('Origin',(0.,-2.,4.));
#9735=CARTESIAN_POINT('',(-1.005,-2.,4.));
#9736=CARTESIAN_POINT('Origin',(0.,-2.,4.));
#9737=CARTESIAN_POINT('Origin',(0.,-1.7,4.));
#9738=CARTESIAN_POINT('',(-1.005,-1.5,4.));
#9739=CARTESIAN_POINT('Origin',(0.,-1.5,4.));
#9740=CARTESIAN_POINT('',(-1.005,-1.7,4.));
#9741=CARTESIAN_POINT('Origin',(0.,-1.7,4.));
#9742=CARTESIAN_POINT('',(-2.4,-1.5,4.));
#9743=CARTESIAN_POINT('Origin',(0.,-1.5,4.));
#9744=CARTESIAN_POINT('',(-2.4,-1.7,4.));
#9745=CARTESIAN_POINT('',(-2.4,-1.7,4.));
#9746=CARTESIAN_POINT('Origin',(0.,-1.7,4.));
#9747=CARTESIAN_POINT('Origin',(0.,-1.5,4.));
#9748=CARTESIAN_POINT('Origin',(0.,-1.7,4.));
#9749=CARTESIAN_POINT('',(0.,0.,0.));
#9750=CARTESIAN_POINT('Origin',(-3.,2.5,0.9));
#9751=CARTESIAN_POINT('',(-3.225,2.5,1.));
#9752=CARTESIAN_POINT('Origin',(-3.,2.5,1.));
#9753=CARTESIAN_POINT('',(-3.225,2.5,1.8));
#9754=CARTESIAN_POINT('',(-3.225,2.5,0.9));
#9755=CARTESIAN_POINT('Origin',(-3.,2.5,1.8));
#9756=CARTESIAN_POINT('Origin',(3.,2.5,0.9));
#9757=CARTESIAN_POINT('',(2.775,2.5,1.));
#9758=CARTESIAN_POINT('Origin',(3.,2.5,1.));
#9759=CARTESIAN_POINT('',(2.775,2.5,1.8));
#9760=CARTESIAN_POINT('',(2.775,2.5,0.9));
#9761=CARTESIAN_POINT('Origin',(3.,2.5,1.8));
#9762=CARTESIAN_POINT('Origin',(-1.4142135623731,1.6,2.58578643762691));
#9763=CARTESIAN_POINT('',(-1.5792135623731,1.7,2.58578643762691));
#9764=CARTESIAN_POINT('Origin',(-1.4142135623731,1.7,2.58578643762691));
#9765=CARTESIAN_POINT('',(-1.5792135623731,3.3,2.58578643762691));
#9766=CARTESIAN_POINT('',(-1.5792135623731,1.6,2.58578643762691));
#9767=CARTESIAN_POINT('Origin',(-1.4142135623731,3.3,2.58578643762691));
#9768=CARTESIAN_POINT('Origin',(-1.41421356237309,1.6,5.41421356237309));
#9769=CARTESIAN_POINT('',(-1.57921356237309,1.7,5.41421356237309));
#9770=CARTESIAN_POINT('Origin',(-1.41421356237309,1.7,5.41421356237309));
#9771=CARTESIAN_POINT('',(-1.57921356237309,3.3,5.41421356237309));
#9772=CARTESIAN_POINT('',(-1.57921356237309,1.6,5.41421356237309));
#9773=CARTESIAN_POINT('Origin',(-1.41421356237309,3.3,5.41421356237309));
#9774=CARTESIAN_POINT('Origin',(1.4142135623731,1.6,5.41421356237309));
#9775=CARTESIAN_POINT('',(1.2492135623731,1.7,5.41421356237309));
#9776=CARTESIAN_POINT('Origin',(1.4142135623731,1.7,5.41421356237309));
#9777=CARTESIAN_POINT('',(1.2492135623731,3.3,5.41421356237309));
#9778=CARTESIAN_POINT('',(1.2492135623731,1.6,5.41421356237309));
#9779=CARTESIAN_POINT('Origin',(1.4142135623731,3.3,5.41421356237309));
#9780=CARTESIAN_POINT('Origin',(1.41421356237309,1.6,2.5857864376269));
#9781=CARTESIAN_POINT('',(1.24921356237309,1.7,2.5857864376269));
#9782=CARTESIAN_POINT('Origin',(1.41421356237309,1.7,2.5857864376269));
#9783=CARTESIAN_POINT('',(1.24921356237309,3.3,2.5857864376269));
#9784=CARTESIAN_POINT('',(1.24921356237309,1.6,2.5857864376269));
#9785=CARTESIAN_POINT('Origin',(1.41421356237309,3.3,2.5857864376269));
#9786=CARTESIAN_POINT('Origin',(0.,1.6,4.));
#9787=CARTESIAN_POINT('',(-1.6,1.7,4.));
#9788=CARTESIAN_POINT('Origin',(0.,1.7,4.));
#9789=CARTESIAN_POINT('',(-1.6,3.3,4.));
#9790=CARTESIAN_POINT('',(-1.6,1.6,4.));
#9791=CARTESIAN_POINT('Origin',(0.,3.3,4.));
#9792=CARTESIAN_POINT('Origin',(-3.6,1.7,1.8));
#9793=CARTESIAN_POINT('',(2.4,1.7,1.8));
#9794=CARTESIAN_POINT('',(2.4,3.3,1.8));
#9795=CARTESIAN_POINT('',(2.4,1.7,1.8));
#9796=CARTESIAN_POINT('',(3.6,1.7,1.8));
#9797=CARTESIAN_POINT('',(3.6,1.7,1.8));
#9798=CARTESIAN_POINT('',(3.6,3.3,1.8));
#9799=CARTESIAN_POINT('',(3.6,1.7,1.8));
#9800=CARTESIAN_POINT('',(3.6,3.3,1.8));
#9801=CARTESIAN_POINT('Origin',(-3.6,1.7,1.8));
#9802=CARTESIAN_POINT('',(-2.4,3.3,1.8));
#9803=CARTESIAN_POINT('',(-2.4,1.7,1.8));
#9804=CARTESIAN_POINT('',(-2.4,2.5,1.8));
#9805=CARTESIAN_POINT('',(-3.6,3.3,1.8));
#9806=CARTESIAN_POINT('',(3.6,3.3,1.8));
#9807=CARTESIAN_POINT('',(-3.6,1.7,1.8));
#9808=CARTESIAN_POINT('',(-3.6,1.7,1.8));
#9809=CARTESIAN_POINT('',(3.6,1.7,1.8));
#9810=CARTESIAN_POINT('Origin',(-3.6,1.7,1.));
#9811=CARTESIAN_POINT('',(-3.6,1.7,1.));
#9812=CARTESIAN_POINT('',(-3.6,1.7,1.8));
#9813=CARTESIAN_POINT('',(-3.6,3.3,1.));
#9814=CARTESIAN_POINT('',(-3.6,3.3,1.8));
#9815=CARTESIAN_POINT('',(-3.6,1.7,1.));
#9816=CARTESIAN_POINT('Origin',(3.6,1.7,1.8));
#9817=CARTESIAN_POINT('',(3.6,1.7,1.));
#9818=CARTESIAN_POINT('',(3.6,1.7,1.));
#9819=CARTESIAN_POINT('',(3.6,3.3,1.));
#9820=CARTESIAN_POINT('',(3.6,1.7,1.));
#9821=CARTESIAN_POINT('',(3.6,3.3,1.));
#9822=CARTESIAN_POINT('Origin',(-2.4,1.7,1.));
#9823=CARTESIAN_POINT('',(2.4,1.7,6.5));
#9824=CARTESIAN_POINT('',(2.4,1.7,1.));
#9825=CARTESIAN_POINT('',(-2.4,1.7,6.5));
#9826=CARTESIAN_POINT('',(-2.4,1.7,6.5));
#9827=CARTESIAN_POINT('',(-2.4,1.7,1.));
#9828=CARTESIAN_POINT('',(-3.6,1.7,1.));
#9829=CARTESIAN_POINT('Origin',(2.4,1.7,1.));
#9830=CARTESIAN_POINT('',(2.4,3.3,6.5));
#9831=CARTESIAN_POINT('',(2.4,3.3,1.));
#9832=CARTESIAN_POINT('',(2.4,1.7,6.5));
#9833=CARTESIAN_POINT('Origin',(2.4,3.3,1.));
#9834=CARTESIAN_POINT('',(-2.4,3.3,6.5));
#9835=CARTESIAN_POINT('',(-2.4,3.3,1.));
#9836=CARTESIAN_POINT('',(2.4,3.3,6.5));
#9837=CARTESIAN_POINT('',(-3.6,3.3,1.));
#9838=CARTESIAN_POINT('Origin',(-2.4,3.3,1.));
#9839=CARTESIAN_POINT('',(-2.4,3.3,6.5));
#9840=CARTESIAN_POINT('Origin',(0.,2.5,6.5));
#9841=CARTESIAN_POINT('Origin',(0.,2.5,1.));
#9842=CARTESIAN_POINT('',(0.,0.,0.));
#9843=CARTESIAN_POINT('Origin',(-1.4142135623731,1.4,2.58578643762691));
#9844=CARTESIAN_POINT('',(-1.6392135623731,1.5,2.58578643762691));
#9845=CARTESIAN_POINT('Origin',(-1.4142135623731,1.5,2.58578643762691));
#9846=CARTESIAN_POINT('',(-1.6392135623731,1.7,2.58578643762691));
#9847=CARTESIAN_POINT('',(-1.6392135623731,1.4,2.58578643762691));
#9848=CARTESIAN_POINT('Origin',(-1.4142135623731,1.7,2.58578643762691));
#9849=CARTESIAN_POINT('Origin',(-1.41421356237309,1.4,5.41421356237309));
#9850=CARTESIAN_POINT('',(-1.6392135623731,1.5,5.41421356237309));
#9851=CARTESIAN_POINT('Origin',(-1.41421356237309,1.5,5.41421356237309));
#9852=CARTESIAN_POINT('',(-1.6392135623731,1.7,5.41421356237309));
#9853=CARTESIAN_POINT('',(-1.6392135623731,1.4,5.41421356237309));
#9854=CARTESIAN_POINT('Origin',(-1.41421356237309,1.7,5.41421356237309));
#9855=CARTESIAN_POINT('Origin',(1.4142135623731,1.4,5.41421356237309));
#9856=CARTESIAN_POINT('',(1.1892135623731,1.5,5.41421356237309));
#9857=CARTESIAN_POINT('Origin',(1.4142135623731,1.5,5.41421356237309));
#9858=CARTESIAN_POINT('',(1.1892135623731,1.7,5.41421356237309));
#9859=CARTESIAN_POINT('',(1.1892135623731,1.4,5.41421356237309));
#9860=CARTESIAN_POINT('Origin',(1.4142135623731,1.7,5.41421356237309));
#9861=CARTESIAN_POINT('Origin',(1.41421356237309,1.4,2.5857864376269));
#9862=CARTESIAN_POINT('',(1.18921356237309,1.5,2.5857864376269));
#9863=CARTESIAN_POINT('Origin',(1.41421356237309,1.5,2.5857864376269));
#9864=CARTESIAN_POINT('',(1.18921356237309,1.7,2.5857864376269));
#9865=CARTESIAN_POINT('',(1.18921356237309,1.4,2.5857864376269));
#9866=CARTESIAN_POINT('Origin',(1.41421356237309,1.7,2.5857864376269));
#9867=CARTESIAN_POINT('Origin',(0.,1.7,4.));
#9868=CARTESIAN_POINT('',(-1.59,2.,4.));
#9869=CARTESIAN_POINT('Origin',(0.,2.,4.));
#9870=CARTESIAN_POINT('',(-1.59,1.7,4.));
#9871=CARTESIAN_POINT('',(-1.59,1.7,4.));
#9872=CARTESIAN_POINT('Origin',(0.,1.7,4.));
#9873=CARTESIAN_POINT('Origin',(0.,2.,4.));
#9874=CARTESIAN_POINT('',(-1.005,2.,4.));
#9875=CARTESIAN_POINT('Origin',(0.,2.,4.));
#9876=CARTESIAN_POINT('Origin',(0.,1.5,4.));
#9877=CARTESIAN_POINT('',(-1.005,1.5,4.));
#9878=CARTESIAN_POINT('',(-1.005,1.5,4.));
#9879=CARTESIAN_POINT('Origin',(0.,1.5,4.));
#9880=CARTESIAN_POINT('Origin',(0.,1.5,4.));
#9881=CARTESIAN_POINT('',(-2.4,1.7,4.));
#9882=CARTESIAN_POINT('Origin',(0.,1.7,4.));
#9883=CARTESIAN_POINT('',(-2.4,1.5,4.));
#9884=CARTESIAN_POINT('',(-2.4,1.5,4.));
#9885=CARTESIAN_POINT('Origin',(0.,1.5,4.));
#9886=CARTESIAN_POINT('Origin',(0.,1.7,4.));
#9887=CARTESIAN_POINT('Origin',(0.,1.5,4.));
#9888=CARTESIAN_POINT('',(0.,0.,0.));
#9889=CARTESIAN_POINT('Origin',(-1.4142135623731,3.2,2.58578643762691));
#9890=CARTESIAN_POINT('',(-1.6392135623731,3.3,2.58578643762691));
#9891=CARTESIAN_POINT('Origin',(-1.4142135623731,3.3,2.58578643762691));
#9892=CARTESIAN_POINT('',(-1.6392135623731,3.5,2.58578643762691));
#9893=CARTESIAN_POINT('',(-1.6392135623731,3.2,2.58578643762691));
#9894=CARTESIAN_POINT('Origin',(-1.4142135623731,3.5,2.58578643762691));
#9895=CARTESIAN_POINT('Origin',(-1.41421356237309,3.2,5.41421356237309));
#9896=CARTESIAN_POINT('',(-1.6392135623731,3.3,5.41421356237309));
#9897=CARTESIAN_POINT('Origin',(-1.41421356237309,3.3,5.41421356237309));
#9898=CARTESIAN_POINT('',(-1.6392135623731,3.5,5.41421356237309));
#9899=CARTESIAN_POINT('',(-1.6392135623731,3.2,5.41421356237309));
#9900=CARTESIAN_POINT('Origin',(-1.41421356237309,3.5,5.41421356237309));
#9901=CARTESIAN_POINT('Origin',(1.4142135623731,3.2,5.41421356237309));
#9902=CARTESIAN_POINT('',(1.1892135623731,3.3,5.41421356237309));
#9903=CARTESIAN_POINT('Origin',(1.4142135623731,3.3,5.41421356237309));
#9904=CARTESIAN_POINT('',(1.1892135623731,3.5,5.41421356237309));
#9905=CARTESIAN_POINT('',(1.1892135623731,3.2,5.41421356237309));
#9906=CARTESIAN_POINT('Origin',(1.4142135623731,3.5,5.41421356237309));
#9907=CARTESIAN_POINT('Origin',(1.41421356237309,3.2,2.5857864376269));
#9908=CARTESIAN_POINT('',(1.18921356237309,3.3,2.5857864376269));
#9909=CARTESIAN_POINT('Origin',(1.41421356237309,3.3,2.5857864376269));
#9910=CARTESIAN_POINT('',(1.18921356237309,3.5,2.5857864376269));
#9911=CARTESIAN_POINT('',(1.18921356237309,3.2,2.5857864376269));
#9912=CARTESIAN_POINT('Origin',(1.41421356237309,3.5,2.5857864376269));
#9913=CARTESIAN_POINT('Origin',(0.,3.,4.));
#9914=CARTESIAN_POINT('',(-1.59,3.3,4.));
#9915=CARTESIAN_POINT('Origin',(0.,3.3,4.));
#9916=CARTESIAN_POINT('',(-1.59,3.,4.));
#9917=CARTESIAN_POINT('',(-1.59,3.,4.));
#9918=CARTESIAN_POINT('Origin',(0.,3.,4.));
#9919=CARTESIAN_POINT('Origin',(0.,3.,4.));
#9920=CARTESIAN_POINT('',(-1.005,3.,4.));
#9921=CARTESIAN_POINT('Origin',(0.,3.,4.));
#9922=CARTESIAN_POINT('Origin',(0.,3.3,4.));
#9923=CARTESIAN_POINT('',(-1.005,3.5,4.));
#9924=CARTESIAN_POINT('Origin',(0.,3.5,4.));
#9925=CARTESIAN_POINT('',(-1.005,3.3,4.));
#9926=CARTESIAN_POINT('Origin',(0.,3.3,4.));
#9927=CARTESIAN_POINT('',(-2.4,3.5,4.));
#9928=CARTESIAN_POINT('Origin',(0.,3.5,4.));
#9929=CARTESIAN_POINT('',(-2.4,3.3,4.));
#9930=CARTESIAN_POINT('',(-2.4,3.3,4.));
#9931=CARTESIAN_POINT('Origin',(0.,3.3,4.));
#9932=CARTESIAN_POINT('Origin',(0.,3.5,4.));
#9933=CARTESIAN_POINT('Origin',(0.,3.3,4.));
#9934=CARTESIAN_POINT('',(0.,0.,0.));
#9935=CARTESIAN_POINT('Origin',(-1.06066017177982,-1.06066017177982,13.2));
#9936=CARTESIAN_POINT('',(-1.22566017177982,-1.06066017177982,13.2));
#9937=CARTESIAN_POINT('Origin',(-1.06066017177982,-1.06066017177982,13.2));
#9938=CARTESIAN_POINT('',(-1.22566017177982,-1.06066017177982,14.));
#9939=CARTESIAN_POINT('',(-1.22566017177982,-1.06066017177982,13.2));
#9940=CARTESIAN_POINT('Origin',(-1.06066017177982,-1.06066017177982,14.));
#9941=CARTESIAN_POINT('Origin',(-1.06066017177982,-1.06066017177982,13.2));
#9942=CARTESIAN_POINT('Origin',(-1.06066017177982,1.06066017177982,13.2));
#9943=CARTESIAN_POINT('',(-1.22566017177982,1.06066017177982,13.2));
#9944=CARTESIAN_POINT('Origin',(-1.06066017177982,1.06066017177982,13.2));
#9945=CARTESIAN_POINT('',(-1.22566017177982,1.06066017177982,14.));
#9946=CARTESIAN_POINT('',(-1.22566017177982,1.06066017177982,13.2));
#9947=CARTESIAN_POINT('Origin',(-1.06066017177982,1.06066017177982,14.));
#9948=CARTESIAN_POINT('Origin',(-1.06066017177982,1.06066017177982,13.2));
#9949=CARTESIAN_POINT('Origin',(1.06066017177982,1.06066017177982,13.2));
#9950=CARTESIAN_POINT('',(0.895660171779821,1.06066017177982,13.2));
#9951=CARTESIAN_POINT('Origin',(1.06066017177982,1.06066017177982,13.2));
#9952=CARTESIAN_POINT('',(0.895660171779821,1.06066017177982,14.));
#9953=CARTESIAN_POINT('',(0.895660171779821,1.06066017177982,13.2));
#9954=CARTESIAN_POINT('Origin',(1.06066017177982,1.06066017177982,14.));
#9955=CARTESIAN_POINT('Origin',(1.06066017177982,1.06066017177982,13.2));
#9956=CARTESIAN_POINT('Origin',(1.06066017177982,-1.06066017177982,13.2));
#9957=CARTESIAN_POINT('',(0.895660171779821,-1.06066017177982,13.2));
#9958=CARTESIAN_POINT('Origin',(1.06066017177982,-1.06066017177982,13.2));
#9959=CARTESIAN_POINT('',(0.895660171779821,-1.06066017177982,14.));
#9960=CARTESIAN_POINT('',(0.895660171779821,-1.06066017177982,13.2));
#9961=CARTESIAN_POINT('Origin',(1.06066017177982,-1.06066017177982,14.));
#9962=CARTESIAN_POINT('Origin',(1.06066017177982,-1.06066017177982,13.2));
#9963=CARTESIAN_POINT('Origin',(0.,0.,10.5));
#9964=CARTESIAN_POINT('',(-1.05,-1.28587913910472E-16,10.5));
#9965=CARTESIAN_POINT('Origin',(0.,0.,10.5));
#9966=CARTESIAN_POINT('',(-1.05,1.28587913910472E-16,14.));
#9967=CARTESIAN_POINT('',(-1.05,-1.28587913910472E-16,10.5));
#9968=CARTESIAN_POINT('Origin',(0.,0.,14.));
#9969=CARTESIAN_POINT('Origin',(0.,0.,10.5));
#9970=CARTESIAN_POINT('',(-0.625,-7.65404249467096E-17,10.5));
#9971=CARTESIAN_POINT('Origin',(0.,0.,10.5));
#9972=CARTESIAN_POINT('Origin',(0.,0.,9.9));
#9973=CARTESIAN_POINT('',(-0.625,-7.65404249467096E-17,10.));
#9974=CARTESIAN_POINT('Origin',(0.,0.,10.));
#9975=CARTESIAN_POINT('',(-0.625,-7.65404249467096E-17,9.9));
#9976=CARTESIAN_POINT('Origin',(3.75,0.,2.4));
#9977=CARTESIAN_POINT('',(3.25,-6.12323399573677E-17,2.4));
#9978=CARTESIAN_POINT('Origin',(3.75,0.,2.4));
#9979=CARTESIAN_POINT('',(3.25,6.12323399573677E-17,14.));
#9980=CARTESIAN_POINT('',(3.25,-6.12323399573677E-17,2.4));
#9981=CARTESIAN_POINT('Origin',(3.75,0.,14.));
#9982=CARTESIAN_POINT('Origin',(3.75,0.,2.4));
#9983=CARTESIAN_POINT('',(3.475,-3.36777869765523E-17,2.4));
#9984=CARTESIAN_POINT('Origin',(3.75,0.,2.4));
#9985=CARTESIAN_POINT('Origin',(3.75,0.,0.9));
#9986=CARTESIAN_POINT('',(3.475,-3.36777869765523E-17,1.));
#9987=CARTESIAN_POINT('Origin',(3.75,0.,1.));
#9988=CARTESIAN_POINT('',(3.475,-3.36777869765523E-17,0.9));
#9989=CARTESIAN_POINT('Origin',(-3.75,0.,2.4));
#9990=CARTESIAN_POINT('',(-4.25,-6.12323399573677E-17,2.4));
#9991=CARTESIAN_POINT('Origin',(-3.75,0.,2.4));
#9992=CARTESIAN_POINT('',(-4.25,6.12323399573677E-17,14.));
#9993=CARTESIAN_POINT('',(-4.25,-6.12323399573677E-17,2.4));
#9994=CARTESIAN_POINT('Origin',(-3.75,0.,14.));
#9995=CARTESIAN_POINT('Origin',(-3.75,0.,2.4));
#9996=CARTESIAN_POINT('',(-4.025,-3.36777869765522E-17,2.4));
#9997=CARTESIAN_POINT('Origin',(-3.75,0.,2.4));
#9998=CARTESIAN_POINT('Origin',(-3.75,0.,0.9));
#9999=CARTESIAN_POINT('',(-4.025,-3.36777869765522E-17,1.));
#10000=CARTESIAN_POINT('Origin',(-3.75,0.,1.));
#10001=CARTESIAN_POINT('',(-4.025,-3.36777869765522E-17,0.9));
#10002=CARTESIAN_POINT('Origin',(4.5,-2.,10.));
#10003=CARTESIAN_POINT('',(-4.5,1.,10.));
#10004=CARTESIAN_POINT('',(-3.,1.,10.));
#10005=CARTESIAN_POINT('',(0.75,1.,10.));
#10006=CARTESIAN_POINT('',(-4.5,2.,10.));
#10007=CARTESIAN_POINT('',(-4.5,-2.,10.));
#10008=CARTESIAN_POINT('',(4.5,2.,10.));
#10009=CARTESIAN_POINT('',(-4.5,2.,10.));
#10010=CARTESIAN_POINT('',(4.5,1.,10.));
#10011=CARTESIAN_POINT('',(4.5,-2.,10.));
#10012=CARTESIAN_POINT('',(3.,1.,10.));
#10013=CARTESIAN_POINT('',(4.125,1.,10.));
#10014=CARTESIAN_POINT('',(3.,-1.,10.));
#10015=CARTESIAN_POINT('',(3.,-1.5,10.));
#10016=CARTESIAN_POINT('',(4.5,-1.,10.));
#10017=CARTESIAN_POINT('',(4.125,-1.,10.));
#10018=CARTESIAN_POINT('',(4.5,-2.,10.));
#10019=CARTESIAN_POINT('',(4.5,-2.,10.));
#10020=CARTESIAN_POINT('',(-4.5,-2.,10.));
#10021=CARTESIAN_POINT('',(-4.5,-2.,10.));
#10022=CARTESIAN_POINT('',(-4.5,-1.,10.));
#10023=CARTESIAN_POINT('',(-4.5,-2.,10.));
#10024=CARTESIAN_POINT('',(-3.,-1.,10.));
#10025=CARTESIAN_POINT('',(0.,-1.,10.));
#10026=CARTESIAN_POINT('',(-3.,-1.5,10.));
#10027=CARTESIAN_POINT('Origin',(0.,2.,12.));
#10028=CARTESIAN_POINT('',(-4.5,2.,14.));
#10029=CARTESIAN_POINT('',(4.5,2.,14.));
#10030=CARTESIAN_POINT('',(4.5,2.,14.));
#10031=CARTESIAN_POINT('',(4.5,2.,10.));
#10032=CARTESIAN_POINT('',(-4.5,2.,14.));
#10033=CARTESIAN_POINT('Origin',(0.,-2.,12.));
#10034=CARTESIAN_POINT('',(4.5,-2.,14.));
#10035=CARTESIAN_POINT('',(-4.5,-2.,14.));
#10036=CARTESIAN_POINT('',(4.5,-2.,14.));
#10037=CARTESIAN_POINT('',(-4.5,-2.,14.));
#10038=CARTESIAN_POINT('',(4.5,-2.,10.));
#10039=CARTESIAN_POINT('Origin',(3.,-1.,1.));
#10040=CARTESIAN_POINT('',(3.,1.,1.));
#10041=CARTESIAN_POINT('',(3.,1.,14.));
#10042=CARTESIAN_POINT('',(3.,-1.,1.));
#10043=CARTESIAN_POINT('',(3.,-1.,1.));
#10044=CARTESIAN_POINT('',(3.,-1.,14.));
#10045=CARTESIAN_POINT('Origin',(3.75,1.,7.5));
#10046=CARTESIAN_POINT('',(4.5,1.,1.));
#10047=CARTESIAN_POINT('',(4.5,1.,1.));
#10048=CARTESIAN_POINT('',(3.,1.,1.));
#10049=CARTESIAN_POINT('Origin',(4.5,-1.,1.));
#10050=CARTESIAN_POINT('',(4.5,-1.,1.));
#10051=CARTESIAN_POINT('',(3.,-1.,1.));
#10052=CARTESIAN_POINT('',(4.5,-1.,1.));
#10053=CARTESIAN_POINT('Origin',(4.5,-1.,14.));
#10054=CARTESIAN_POINT('',(4.5,-1.,1.));
#10055=CARTESIAN_POINT('',(4.5,-1.,14.));
#10056=CARTESIAN_POINT('Origin',(3.75,-1.,7.5));
#10057=CARTESIAN_POINT('Origin',(-3.,-1.,1.));
#10058=CARTESIAN_POINT('',(-3.,-1.,1.));
#10059=CARTESIAN_POINT('',(-3.,-1.,1.));
#10060=CARTESIAN_POINT('',(-3.,1.,1.));
#10061=CARTESIAN_POINT('',(-3.,-1.,1.));
#10062=CARTESIAN_POINT('',(-3.,1.,1.));
#10063=CARTESIAN_POINT('Origin',(-4.5,-1.,1.));
#10064=CARTESIAN_POINT('',(-4.5,-1.,1.));
#10065=CARTESIAN_POINT('',(-4.5,-1.,1.));
#10066=CARTESIAN_POINT('',(-4.5,-1.,1.));
#10067=CARTESIAN_POINT('Origin',(-3.,1.,1.));
#10068=CARTESIAN_POINT('',(-4.5,1.,1.));
#10069=CARTESIAN_POINT('',(-3.,1.,1.));
#10070=CARTESIAN_POINT('',(-4.5,1.,1.));
#10071=CARTESIAN_POINT('Origin',(-4.5,1.,1.));
#10072=CARTESIAN_POINT('',(-4.5,1.,1.));
#10073=CARTESIAN_POINT('',(-4.5,-2.,14.));
#10074=CARTESIAN_POINT('Origin',(-3.75,0.,14.));
#10075=CARTESIAN_POINT('Origin',(-3.75,0.,1.));
#10076=CARTESIAN_POINT('',(0.,0.,0.));
#10077=CARTESIAN_POINT('Origin',(-1.06066017177982,-1.06066017177982,13.9));
#10078=CARTESIAN_POINT('',(-1.28566017177982,-1.06066017177982,14.));
#10079=CARTESIAN_POINT('Origin',(-1.06066017177982,-1.06066017177982,14.));
#10080=CARTESIAN_POINT('',(-1.28566017177982,-1.06066017177982,14.4));
#10081=CARTESIAN_POINT('',(-1.28566017177982,-1.06066017177982,13.9));
#10082=CARTESIAN_POINT('Origin',(-1.06066017177982,-1.06066017177982,14.4));
#10083=CARTESIAN_POINT('Origin',(-1.06066017177982,1.06066017177982,13.9));
#10084=CARTESIAN_POINT('',(-1.28566017177982,1.06066017177982,14.));
#10085=CARTESIAN_POINT('Origin',(-1.06066017177982,1.06066017177982,14.));
#10086=CARTESIAN_POINT('',(-1.28566017177982,1.06066017177982,14.4));
#10087=CARTESIAN_POINT('',(-1.28566017177982,1.06066017177982,13.9));
#10088=CARTESIAN_POINT('Origin',(-1.06066017177982,1.06066017177982,14.4));
#10089=CARTESIAN_POINT('Origin',(1.06066017177982,1.06066017177982,13.9));
#10090=CARTESIAN_POINT('',(0.835660171779821,1.06066017177982,14.));
#10091=CARTESIAN_POINT('Origin',(1.06066017177982,1.06066017177982,14.));
#10092=CARTESIAN_POINT('',(0.835660171779821,1.06066017177982,14.4));
#10093=CARTESIAN_POINT('',(0.835660171779821,1.06066017177982,13.9));
#10094=CARTESIAN_POINT('Origin',(1.06066017177982,1.06066017177982,14.4));
#10095=CARTESIAN_POINT('Origin',(1.06066017177982,-1.06066017177982,13.9));
#10096=CARTESIAN_POINT('',(0.835660171779821,-1.06066017177982,14.));
#10097=CARTESIAN_POINT('Origin',(1.06066017177982,-1.06066017177982,14.));
#10098=CARTESIAN_POINT('',(0.835660171779821,-1.06066017177982,14.4));
#10099=CARTESIAN_POINT('',(0.835660171779821,-1.06066017177982,13.9));
#10100=CARTESIAN_POINT('Origin',(1.06066017177982,-1.06066017177982,14.4));
#10101=CARTESIAN_POINT('Origin',(0.,0.,13.5));
#10102=CARTESIAN_POINT('',(-1.04,-1.27363267111325E-16,14.));
#10103=CARTESIAN_POINT('Origin',(0.,0.,14.));
#10104=CARTESIAN_POINT('',(-1.04,-1.27363267111325E-16,13.5));
#10105=CARTESIAN_POINT('',(-1.04,-1.27363267111325E-16,13.5));
#10106=CARTESIAN_POINT('Origin',(0.,0.,13.5));
#10107=CARTESIAN_POINT('Origin',(0.,0.,13.5));
#10108=CARTESIAN_POINT('',(-0.625,-7.65404249467096E-17,13.5));
#10109=CARTESIAN_POINT('Origin',(0.,0.,13.5));
#10110=CARTESIAN_POINT('Origin',(0.,0.,14.));
#10111=CARTESIAN_POINT('',(-0.625,-7.65404249467096E-17,14.4));
#10112=CARTESIAN_POINT('Origin',(0.,0.,14.4));
#10113=CARTESIAN_POINT('',(-0.625,-7.65404249467096E-17,14.));
#10114=CARTESIAN_POINT('Origin',(0.,0.,14.));
#10115=CARTESIAN_POINT('',(-1.8,-2.20436423846524E-16,14.4));
#10116=CARTESIAN_POINT('Origin',(0.,0.,14.4));
#10117=CARTESIAN_POINT('',(-1.8,-2.20436423846524E-16,14.));
#10118=CARTESIAN_POINT('',(-1.8,-2.20436423846524E-16,14.));
#10119=CARTESIAN_POINT('Origin',(0.,0.,14.));
#10120=CARTESIAN_POINT('Origin',(0.,0.,14.4));
#10121=CARTESIAN_POINT('Origin',(0.,0.,14.));
#10122=CARTESIAN_POINT('',(0.,0.,0.));
#10123=CARTESIAN_POINT('Ctrl Pts',(0.999999575810999,0.00315098358513781,
7.20006622055264));
#10124=CARTESIAN_POINT('Ctrl Pts',(0.999974319608277,0.190760468856422,
7.20795524501636));
#10125=CARTESIAN_POINT('Ctrl Pts',(0.892344234443071,0.564401735476683,
7.22374165130483));
#10126=CARTESIAN_POINT('Ctrl Pts',(0.456170863303355,0.954569139239392,
7.24746551842362));
#10127=CARTESIAN_POINT('Ctrl Pts',(-0.121643296695006,1.0527111229517,7.27123039275792));
#10128=CARTESIAN_POINT('Ctrl Pts',(-0.664174499114347,0.828146653873478,
7.29503750827097));
#10129=CARTESIAN_POINT('Ctrl Pts',(-1.00466229107333,0.348451955041142,
7.31888617441183));
#10130=CARTESIAN_POINT('Ctrl Pts',(-1.03783821085617,-0.239862803165599,
7.34277653444097));
#10131=CARTESIAN_POINT('Ctrl Pts',(-0.752436914310739,-0.756562482852077,
7.36670833282365));
#10132=CARTESIAN_POINT('Ctrl Pts',(-0.234997931414651,-1.04270891419437,
7.39068146490982));
#10133=CARTESIAN_POINT('Ctrl Pts',(0.356377432582172,-1.00964746384867,
7.41469572763747));
#10134=CARTESIAN_POINT('Ctrl Pts',(0.840341677037224,-0.666437865062604,
7.43875093208249));
#10135=CARTESIAN_POINT('Ctrl Pts',(1.06790358406505,-0.117422164195028,
7.4628468515188));
#10136=CARTESIAN_POINT('Ctrl Pts',(0.968336509361683,0.469494166098508,
7.48698324256581));
#10137=CARTESIAN_POINT('Ctrl Pts',(0.571081336399399,0.914217869413367,
7.51115983904362));
#10138=CARTESIAN_POINT('Ctrl Pts',(-0.00276942901145937,1.07968430615977,
7.53537635143244));
#10139=CARTESIAN_POINT('Ctrl Pts',(-0.577781503135752,0.914223804149117,
7.55963247041146));
#10140=CARTESIAN_POINT('Ctrl Pts',(-0.962145622562424,0.483976677731404,
7.58302803095162));
#10141=CARTESIAN_POINT('Ctrl Pts',(-1.07125753086067,-0.0562794445165808,
7.60555779623404));
#10142=CARTESIAN_POINT('Ctrl Pts',(-0.915194862614763,-0.562561634031091,
7.6272168563822));
#10143=CARTESIAN_POINT('Ctrl Pts',(-0.53551487530705,-0.932963762094015,
7.64890612590553));
#10144=CARTESIAN_POINT('Ctrl Pts',(-0.024035065806305,-1.07736876663697,
7.67062531437742));
#10145=CARTESIAN_POINT('Ctrl Pts',(0.494146757015346,-0.958466814289234,
7.69237411680017));
#10146=CARTESIAN_POINT('Ctrl Pts',(0.961479539986573,-0.548279772601945,
7.71778190065853));
#10147=CARTESIAN_POINT('Ctrl Pts',(1.12756301652098,0.172482400610549,7.74686765103336));
#10148=CARTESIAN_POINT('Ctrl Pts',(0.75611713355168,0.813684959589575,7.77601030696451));
#10149=CARTESIAN_POINT('Ctrl Pts',(0.185875815215743,1.06965010757807,7.80155082448588));
#10150=CARTESIAN_POINT('Ctrl Pts',(-0.348517058347165,1.02984652160674,
7.82347022110603));
#10151=CARTESIAN_POINT('Ctrl Pts',(-0.761949296282463,0.762592777124389,
7.84358787235736));
#10152=CARTESIAN_POINT('Ctrl Pts',(-0.996722963062006,0.388518849169714,
7.86189613571743));
#10153=CARTESIAN_POINT('Ctrl Pts',(-1.07098690831041,-0.00260829917091459,
7.87838843437341));
#10154=CARTESIAN_POINT('Ctrl Pts',(-0.99661183226746,-0.393594984460838,
7.894895410549));
#10155=CARTESIAN_POINT('Ctrl Pts',(-0.714908576434247,-0.844892296878379,
7.9169240469514));
#10156=CARTESIAN_POINT('Ctrl Pts',(-0.084422651145012,-1.14985023564212,
7.94449562780488));
#10157=CARTESIAN_POINT('Ctrl Pts',(0.721887320494981,-0.901498071462995,
7.97763725360595));
#10158=CARTESIAN_POINT('Ctrl Pts',(1.14390600676876,-0.170383526932712,
8.01083302661308));
#10159=CARTESIAN_POINT('Ctrl Pts',(0.956311918053777,0.65401391794098,8.04408130906187));
#10160=CARTESIAN_POINT('Ctrl Pts',(0.25602906697655,1.13176193513965,8.07738040653961));
#10161=CARTESIAN_POINT('Ctrl Pts',(-0.488510543500641,1.01860423556296,
8.10702323570327));
#10162=CARTESIAN_POINT('Ctrl Pts',(-0.942716248260153,0.573655629467007,
8.13299136011509));
#10163=CARTESIAN_POINT('Ctrl Pts',(-1.10358636285334,0.0534364176198665,
8.15527022722507));
#10164=CARTESIAN_POINT('Ctrl Pts',(-0.99543872479676,-0.481361877750802,
8.17756901902506));
#10165=CARTESIAN_POINT('Ctrl Pts',(-0.644826641417894,-0.899786909633448,
8.1998871769012));
#10166=CARTESIAN_POINT('Ctrl Pts',(-0.263312902512338,-1.04918995788175,
8.21663989380025));
#10167=CARTESIAN_POINT('Ctrl Pts',(0.00166665731618679,-1.0655343402046,
8.22781406534667));
#10168=CARTESIAN_POINT('Ctrl Pts',(0.178270288589001,-1.05454413855026,
8.23526501957515));
#10169=CARTESIAN_POINT('Ctrl Pts',(0.437439999691742,-0.98876491629653,
8.24644481283225));
#10170=CARTESIAN_POINT('Ctrl Pts',(0.741357296669408,-0.797196125183601,
8.26135855011107));
#10171=CARTESIAN_POINT('Ctrl Pts',(1.06427742047819,-0.363196133741635,
8.28374205636937));
#10172=CARTESIAN_POINT('Ctrl Pts',(1.1191132547847,0.345488423812591,8.31174498186711));
#10173=CARTESIAN_POINT('Ctrl Pts',(0.584140656179565,1.01596202851522,8.34538413710338));
#10174=CARTESIAN_POINT('Ctrl Pts',(-0.19096844855633,1.13165287559935,8.37625078730322));
#10175=CARTESIAN_POINT('Ctrl Pts',(-0.797411359462935,0.795301993540907,
8.40433431031039));
#10176=CARTESIAN_POINT('Ctrl Pts',(-1.0990783559073,0.250015446968417,8.4296262708737));
#10177=CARTESIAN_POINT('Ctrl Pts',(-1.06426569125542,-0.373802040240765,
8.45493410201599));
#10178=CARTESIAN_POINT('Ctrl Pts',(-0.769553388901587,-0.788092512102153,
8.47556748693345));
#10179=CARTESIAN_POINT('Ctrl Pts',(-0.367608264833719,-1.03377453912702,
8.49527086803642));
#10180=CARTESIAN_POINT('Ctrl Pts',(0.0389894662197936,-1.10568483145998,
8.51216552927169));
#10181=CARTESIAN_POINT('Ctrl Pts',(0.476842798425807,-0.987859734068039,
8.53094473644388));
#10182=CARTESIAN_POINT('Ctrl Pts',(0.805101130351003,-0.7459169684144,8.54785141982868));
#10183=CARTESIAN_POINT('Ctrl Pts',(1.02206224073455,-0.400294829517718,
8.56476322077897));
#10184=CARTESIAN_POINT('Ctrl Pts',(1.11108597940432,0.0676090739442989,
8.58449929513004));
#10185=CARTESIAN_POINT('Ctrl Pts',(0.957486327179168,0.602305552598091,
8.60706239241156));
#10186=CARTESIAN_POINT('Ctrl Pts',(0.490319176226327,1.0196961225561,8.63245514939238));
#10187=CARTESIAN_POINT('Ctrl Pts',(-0.127227772869885,1.12465246691674,
8.65785621578684));
#10188=CARTESIAN_POINT('Ctrl Pts',(-0.706252354762176,0.884861784560879,
8.6832646175365));
#10189=CARTESIAN_POINT('Ctrl Pts',(-1.06898139570907,0.373646110671472,
8.70867937640931));
#10190=CARTESIAN_POINT('Ctrl Pts',(-1.10415883703196,-0.252336062683339,
8.73409951326223));
#10191=CARTESIAN_POINT('Ctrl Pts',(-0.800834752831557,-0.801177522527246,
8.75952404569165));
#10192=CARTESIAN_POINT('Ctrl Pts',(-0.251930241323733,-1.10455619700772,
8.78495198825788));
#10193=CARTESIAN_POINT('Ctrl Pts',(0.374309533721303,-1.06939244573458,
8.81038235029736));
#10194=CARTESIAN_POINT('Ctrl Pts',(0.88588373813812,-0.706416051605379,
8.83581414648952));
#10195=CARTESIAN_POINT('Ctrl Pts',(1.12593002076033,-0.126889341474946,
8.86124638643539));
#10196=CARTESIAN_POINT('Ctrl Pts',(1.02087104515559,0.491507891337351,8.88667807898767));
#10197=CARTESIAN_POINT('Ctrl Pts',(0.602911335681679,0.959196578831539,
8.91210823370906));
#10198=CARTESIAN_POINT('Ctrl Pts',(0.000316973456126708,1.13280882473463,
8.93753586563178));
#10199=CARTESIAN_POINT('Ctrl Pts',(-0.602311983560242,0.959240722445107,
8.9629599838141));
#10200=CARTESIAN_POINT('Ctrl Pts',(-1.00436822137552,0.509038661422071,
8.98743813657581));
#10201=CARTESIAN_POINT('Ctrl Pts',(-1.11811011681427,-0.0552669144060651,
9.01097002817133));
#10202=CARTESIAN_POINT('Ctrl Pts',(-0.955644771077333,-0.583087731975911,
9.03355562561233));
#10203=CARTESIAN_POINT('Ctrl Pts',(-0.593074356957321,-0.936728146430118,
9.0542538609391));
#10204=CARTESIAN_POINT('Ctrl Pts',(-0.164731041598437,-1.08578943530602,
9.07306578079699));
#10205=CARTESIAN_POINT('Ctrl Pts',(0.380219776536112,-1.06693040182505,
9.09563491033651));
#10206=CARTESIAN_POINT('Ctrl Pts',(0.853779549938941,-0.745621203287222,
9.11819570154211));
#10207=CARTESIAN_POINT('Ctrl Pts',(1.06953462325323,-0.245092836305948,
9.14074702398398));
#10208=CARTESIAN_POINT('Ctrl Pts',(1.09185195352203,0.298202592837182,9.16329164905568));
#10209=CARTESIAN_POINT('Ctrl Pts',(0.734297058725123,0.919425032182445,
9.19145918094331));
#10210=CARTESIAN_POINT('Ctrl Pts',(0.0501860572080287,1.12913650428628,
9.21960716991184));
#10211=CARTESIAN_POINT('Ctrl Pts',(-0.47422284767955,0.986938013732599,
9.24211273100823));
#10212=CARTESIAN_POINT('Ctrl Pts',(-0.83834294439581,0.718994011703782,
9.26085993499593));
#10213=CARTESIAN_POINT('Ctrl Pts',(-1.0797140885543,0.276058653254629,9.28147192866405));
#10214=CARTESIAN_POINT('Ctrl Pts',(-1.0792869722179,-0.273490761429736,
9.30394472055128));
#10215=CARTESIAN_POINT('Ctrl Pts',(-0.816874083948392,-0.756154521252702,
9.32640385818033));
#10216=CARTESIAN_POINT('Ctrl Pts',(-0.355458797527567,-1.05362205517351,
9.34884870640624));
#10217=CARTESIAN_POINT('Ctrl Pts',(0.191577194376755,-1.09493860698716,
9.37127864639074));
#10218=CARTESIAN_POINT('Ctrl Pts',(0.571484722667441,-0.923210767165354,
9.38832293897591));
#10219=CARTESIAN_POINT('Ctrl Pts',(0.775578610165073,-0.735373724461368,
9.39999172743641));
#10220=CARTESIAN_POINT('Ctrl Pts',(0.90219668945127,-0.581077610283799,
9.40839153478326));
#10221=CARTESIAN_POINT('Ctrl Pts',(1.06423218001646,-0.268505675241936,
9.42308663622534));
#10222=CARTESIAN_POINT('Ctrl Pts',(1.08737574685665,0.14445700622961,9.43987039483926));
#10223=CARTESIAN_POINT('Ctrl Pts',(0.943512119332504,0.519555849049532,
9.45664308969273));
#10224=CARTESIAN_POINT('Ctrl Pts',(0.702595952885493,0.840663912121189,
9.47340826939813));
#10225=CARTESIAN_POINT('Ctrl Pts',(0.250731034525726,1.09066378632527,9.49435038976507));
#10226=CARTESIAN_POINT('Ctrl Pts',(-0.367646366337481,1.05577469318307,
9.51945715090945));
#10227=CARTESIAN_POINT('Ctrl Pts',(-0.872073427555176,0.697769149747224,
9.54453931621249));
#10228=CARTESIAN_POINT('Ctrl Pts',(-1.10851395153864,0.126754498956172,
9.56959609551394));
#10229=CARTESIAN_POINT('Ctrl Pts',(-1.004997965557,-0.481859237919703,9.59462670660628));
#10230=CARTESIAN_POINT('Ctrl Pts',(-0.593994937248818,-0.94163509404227,
9.61963038098806));
#10231=CARTESIAN_POINT('Ctrl Pts',(-0.0020235655980388,-1.11207375119343,
9.6446063758667));
#10232=CARTESIAN_POINT('Ctrl Pts',(0.589215999041395,-0.941636436533483,
9.66955394755264));
#10233=CARTESIAN_POINT('Ctrl Pts',(0.99867475328867,-0.483298149068583,
9.69447238340543));
#10234=CARTESIAN_POINT('Ctrl Pts',(1.10139617547556,0.121906639873499,9.71936097538517));
#10235=CARTESIAN_POINT('Ctrl Pts',(0.866669607038716,0.688301956936916,
9.74421904187644));
#10236=CARTESIAN_POINT('Ctrl Pts',(0.367204775824758,1.0425526426198,9.76904590972932));
#10237=CARTESIAN_POINT('Ctrl Pts',(-0.243395435261487,1.07672488055471,
9.79384092765142));
#10238=CARTESIAN_POINT('Ctrl Pts',(-0.777888567237211,0.781186417289152,
9.81860345995005));
#10239=CARTESIAN_POINT('Ctrl Pts',(-1.07283036518199,0.247282943918733,
9.84333289822209));
#10240=CARTESIAN_POINT('Ctrl Pts',(-1.03856704754786,-0.360866232625645,
9.86802861303319));
#10241=CARTESIAN_POINT('Ctrl Pts',(-0.686501281653619,-0.856920605922548,
9.892690097101));
#10242=CARTESIAN_POINT('Ctrl Pts',(-0.125304938207573,-1.08924443021579,
9.91731661435472));
#10243=CARTESIAN_POINT('Ctrl Pts',(0.472593334675849,-0.987703022851267,
9.94190800522239));
#10244=CARTESIAN_POINT('Ctrl Pts',(0.924078607982629,-0.583894056083662,
9.9664628819065));
#10245=CARTESIAN_POINT('Ctrl Pts',(1.03553205098759,-0.196980695813872,
9.98281022139497));
#10246=CARTESIAN_POINT('Ctrl Pts',(1.03555819462295,-0.00277911247133682,
9.99097644525911));
#10247=CARTESIAN_POINT('Ctrl Pts',(0.977559628488695,0.00314796269385491,
7.20006622055264));
#10248=CARTESIAN_POINT('Ctrl Pts',(0.977534931919559,0.186600347624405,
7.20778043793643));
#10249=CARTESIAN_POINT('Ctrl Pts',(0.872326621716519,0.551848843788545,
7.22321134603222));
#10250=CARTESIAN_POINT('Ctrl Pts',(0.445888516650333,0.933334827963534,
7.24640607517782));
#10251=CARTESIAN_POINT('Ctrl Pts',(-0.119073548305639,1.02929389999416,
7.26964128868359));
#10252=CARTESIAN_POINT('Ctrl Pts',(-0.649587147996202,0.80971547210797,
7.29292023194622));
#10253=CARTESIAN_POINT('Ctrl Pts',(-0.982569682264781,0.340608289962485,
7.31624170699604));
#10254=CARTESIAN_POINT('Ctrl Pts',(-1.01502761301115,-0.234786092628464,
7.33960648723202));
#10255=CARTESIAN_POINT('Ctrl Pts',(-0.735871175247769,-0.740204838677808,
7.36301444474564));
#10256=CARTESIAN_POINT('Ctrl Pts',(-0.229676322236327,-1.02014816093488,
7.3864658304475));
#10257=CARTESIAN_POINT('Ctrl Pts',(0.348937939981405,-0.987814457701798,
7.4099606987694));
#10258=CARTESIAN_POINT('Ctrl Pts',(0.822539330220122,-0.651972394453966,
7.43349915759815));
#10259=CARTESIAN_POINT('Ctrl Pts',(1.04527595941213,-0.114640290127698,
7.45708126355647));
#10260=CARTESIAN_POINT('Ctrl Pts',(0.947826468806296,0.459896400546727,
7.48070704898826));
#10261=CARTESIAN_POINT('Ctrl Pts',(0.55889347637454,0.895331088517642,7.50437654814852));
#10262=CARTESIAN_POINT('Ctrl Pts',(-0.00306079128538847,1.05738788811831,
7.52808969478327));
#10263=CARTESIAN_POINT('Ctrl Pts',(-0.566280527706047,0.895342454830755,
7.55184656451516));
#10264=CARTESIAN_POINT('Ctrl Pts',(-0.94285566098478,0.473846121224849,
7.57476532068617));
#10265=CARTESIAN_POINT('Ctrl Pts',(-1.0497916614659,-0.0555531181652621,
7.59684113555968));
#10266=CARTESIAN_POINT('Ctrl Pts',(-0.896848267782611,-0.551773383072111,
7.6180679179377));
#10267=CARTESIAN_POINT('Ctrl Pts',(-0.524644889084921,-0.914897925677014,
7.63932924215096));
#10268=CARTESIAN_POINT('Ctrl Pts',(-0.0231086211666074,-1.0565167949332,
7.66062527908679));
#10269=CARTESIAN_POINT('Ctrl Pts',(0.485127965286644,-0.939908247511382,
7.6819553795526));
#10270=CARTESIAN_POINT('Ctrl Pts',(0.943615377154503,-0.537522345290259,
7.70687961457021));
#10271=CARTESIAN_POINT('Ctrl Pts',(1.10664549720515,0.169763989700331,7.73541865071932));
#10272=CARTESIAN_POINT('Ctrl Pts',(0.742051547502606,0.79926014258511,7.76402418077492));
#10273=CARTESIAN_POINT('Ctrl Pts',(0.1820386242008,1.05066099789059,7.78910535841451));
#10274=CARTESIAN_POINT('Ctrl Pts',(-0.342925213792071,1.01157659627672,
7.81063708262925));
#10275=CARTESIAN_POINT('Ctrl Pts',(-0.749174696900719,0.748993162117811,
7.83040267717073));
#10276=CARTESIAN_POINT('Ctrl Pts',(-0.979935807647696,0.381329024216996,
7.84839633933116));
#10277=CARTESIAN_POINT('Ctrl Pts',(-1.05295127075641,-0.0031834724715258,
7.86460871683656));
#10278=CARTESIAN_POINT('Ctrl Pts',(-0.979823859029814,-0.387650529628831,
7.88083924305493));
#10279=CARTESIAN_POINT('Ctrl Pts',(-0.702763365403678,-0.831532214326253,
7.9025045281952));
#10280=CARTESIAN_POINT('Ctrl Pts',(-0.0824799953521556,-1.13161645631995,
7.92962705663339));
#10281=CARTESIAN_POINT('Ctrl Pts',(0.711242926121418,-0.887223370319477,
7.9622469399467));
#10282=CARTESIAN_POINT('Ctrl Pts',(1.12693381986534,-0.167219554477753,
7.99493570676171));
#10283=CARTESIAN_POINT('Ctrl Pts',(0.942170158410588,0.645122540676551,
8.02769289174508));
#10284=CARTESIAN_POINT('Ctrl Pts',(0.251833448908431,1.11619302546554,8.06051740773355));
#10285=CARTESIAN_POINT('Ctrl Pts',(-0.482576734552971,1.00466065240982,
8.08975175083041));
#10286=CARTESIAN_POINT('Ctrl Pts',(-0.930837186086348,0.565588449238039,
8.1153761207135));
#10287=CARTESIAN_POINT('Ctrl Pts',(-1.08967697962172,0.0520404847636478,
8.13736727171514));
#10288=CARTESIAN_POINT('Ctrl Pts',(-0.982903963949899,-0.476104949614679,
8.15938616711863));
#10289=CARTESIAN_POINT('Ctrl Pts',(-0.636540954845654,-0.889508172876264,
8.18143408833578));
#10290=CARTESIAN_POINT('Ctrl Pts',(-0.259505287977444,-1.03717085636039,
8.1979881155864));
#10291=CARTESIAN_POINT('Ctrl Pts',(0.00245412741644389,-1.05333143683712,
8.20903477211785));
#10292=CARTESIAN_POINT('Ctrl Pts',(0.177059177795229,-1.04246573347879,
8.21640112872543));
#10293=CARTESIAN_POINT('Ctrl Pts',(0.433327913156591,-0.977427600945312,
8.22745510314132));
#10294=CARTESIAN_POINT('Ctrl Pts',(0.73391120866048,-0.78797120607176,8.2422033360845));
#10295=CARTESIAN_POINT('Ctrl Pts',(1.05339268942341,-0.358614771787532,
8.26434632322957));
#10296=CARTESIAN_POINT('Ctrl Pts',(1.10774289737246,0.342815554655969,8.29206074311086));
#10297=CARTESIAN_POINT('Ctrl Pts',(0.578013407396415,1.00685700818336,8.32536809202379));
#10298=CARTESIAN_POINT('Ctrl Pts',(-0.190065697378914,1.12158925721513,
8.35595007218663));
#10299=CARTESIAN_POINT('Ctrl Pts',(-0.791379955781598,0.788136209353913,
8.38379141767993));
#10300=CARTESIAN_POINT('Ctrl Pts',(-1.09065818214293,0.247264712325509,
8.40887610904288));
#10301=CARTESIAN_POINT('Ctrl Pts',(-1.05615602025911,-0.371820083200091,
8.43398889502081));
#10302=CARTESIAN_POINT('Ctrl Pts',(-0.763582331280387,-0.783164528531196,
8.45447107190819));
#10303=CARTESIAN_POINT('Ctrl Pts',(-0.364356836371496,-1.02719384800769,
8.47404015218794));
#10304=CARTESIAN_POINT('Ctrl Pts',(0.0396184639487176,-1.0986608375699,
8.49082507049449));
#10305=CARTESIAN_POINT('Ctrl Pts',(0.4747993472484,-0.981570587611574,8.5094874174984));
#10306=CARTESIAN_POINT('Ctrl Pts',(0.801179445412529,-0.741029716701455,
8.52629619867346));
#10307=CARTESIAN_POINT('Ctrl Pts',(1.01695965272321,-0.397307355171047,
8.54311315644057));
#10308=CARTESIAN_POINT('Ctrl Pts',(1.10554233979669,0.0681936417011055,
8.56274660530892));
#10309=CARTESIAN_POINT('Ctrl Pts',(0.952705524054136,0.600346322280504,
8.5851983552402));
#10310=CARTESIAN_POINT('Ctrl Pts',(0.487557651772792,1.01598809297735,8.61047974857097));
#10311=CARTESIAN_POINT('Ctrl Pts',(-0.127651652476803,1.12058418421206,
8.63578130248315));
#10312=CARTESIAN_POINT('Ctrl Pts',(-0.70478866362112,0.881619626848855,
8.66110291473919));
#10313=CARTESIAN_POINT('Ctrl Pts',(-1.06653738915564,0.371858090305246,
8.68644322194209));
#10314=CARTESIAN_POINT('Ctrl Pts',(-1.10167663567818,-0.252676170428594,
8.71180143479237));
#10315=CARTESIAN_POINT('Ctrl Pts',(-0.798942597498512,-0.800540151616223,
8.73717650800646));
#10316=CARTESIAN_POINT('Ctrl Pts',(-0.25078864090532,-1.10355366139075,
8.76256750487144));
#10317=CARTESIAN_POINT('Ctrl Pts',(0.374929053613694,-1.0684625769043,8.7879734299407));
#10318=CARTESIAN_POINT('Ctrl Pts',(0.886351621064952,-0.705646605063887,
8.81339330544931));
#10319=CARTESIAN_POINT('Ctrl Pts',(1.12647324119551,-0.126050893654806,
8.83882613969898));
#10320=CARTESIAN_POINT('Ctrl Pts',(1.02139014639355,0.492749598489448,8.86427091353165));
#10321=CARTESIAN_POINT('Ctrl Pts',(0.602990734075153,0.960997323753939,
8.88972664071518));
#10322=CARTESIAN_POINT('Ctrl Pts',(-0.000567847562754408,1.13493523731139,
8.91519221987827));
#10323=CARTESIAN_POINT('Ctrl Pts',(-0.604479916359356,0.9610454826922,8.94066675637306));
#10324=CARTESIAN_POINT('Ctrl Pts',(-1.00761036182794,0.5097064617892,8.96520501612694));
#10325=CARTESIAN_POINT('Ctrl Pts',(-1.12172878107286,-0.0563180902115076,
8.98880606838067));
#10326=CARTESIAN_POINT('Ctrl Pts',(-0.958723063179525,-0.586004022927428,
9.01146964038096));
#10327=CARTESIAN_POINT('Ctrl Pts',(-0.59474503181829,-0.941054468652076,
9.03224747251221));
#10328=CARTESIAN_POINT('Ctrl Pts',(-0.164564414600358,-1.09076932470309,
9.05113813987772));
#10329=CARTESIAN_POINT('Ctrl Pts',(0.382914792126433,-1.0718353554875,9.07381083702006));
#10330=CARTESIAN_POINT('Ctrl Pts',(0.858914210761414,-0.7489475446806,9.09648289188614));
#10331=CARTESIAN_POINT('Ctrl Pts',(1.07589051190367,-0.245617047231296,
9.1191583368655));
#10332=CARTESIAN_POINT('Ctrl Pts',(1.09835720626968,0.300895372898752,9.14183499997529));
#10333=CARTESIAN_POINT('Ctrl Pts',(0.738597876638515,0.926101901793705,
9.1701764747506));
#10334=CARTESIAN_POINT('Ctrl Pts',(0.0497353559870152,1.13736148182463,
9.19851634662638));
#10335=CARTESIAN_POINT('Ctrl Pts',(-0.478615212533917,0.994112255401606,
9.22118869187345));
#10336=CARTESIAN_POINT('Ctrl Pts',(-0.845581735917551,0.72408762970704,
9.24008098535963));
#10337=CARTESIAN_POINT('Ctrl Pts',(-1.08894413293595,0.27757420396775,9.26085707574209));
#10338=CARTESIAN_POINT('Ctrl Pts',(-1.08853511612709,-0.276687817589094,
9.28352144802081));
#10339=CARTESIAN_POINT('Ctrl Pts',(-0.823804291843437,-0.763690543375918,
9.30617985595382));
#10340=CARTESIAN_POINT('Ctrl Pts',(-0.358084308708253,-1.06395939160588,
9.32883258019174));
#10341=CARTESIAN_POINT('Ctrl Pts',(0.19429771997621,-1.10571128876695,9.35148111779932));
#10342=CARTESIAN_POINT('Ctrl Pts',(0.578041077184206,-0.932257994507511,
9.36869420639422));
#10343=CARTESIAN_POINT('Ctrl Pts',(0.784267005411894,-0.742459747249929,
9.38048462316672));
#10344=CARTESIAN_POINT('Ctrl Pts',(0.912220806450212,-0.586536627035717,
9.38897270741444));
#10345=CARTESIAN_POINT('Ctrl Pts',(1.0759938553963,-0.270623175475007,9.40382440993621));
#10346=CARTESIAN_POINT('Ctrl Pts',(1.09941116997266,0.146857322783328,9.42078900879545));
#10347=CARTESIAN_POINT('Ctrl Pts',(0.953919265860187,0.526219027318657,
9.43775151843459));
#10348=CARTESIAN_POINT('Ctrl Pts',(0.710221272720023,0.851041504230473,
9.45470967792948));
#10349=CARTESIAN_POINT('Ctrl Pts',(0.253020054731783,1.10402529591777,9.47589728129195));
#10350=CARTESIAN_POINT('Ctrl Pts',(-0.372954067823897,1.06874219751822,
9.50131022193773));
#10351=CARTESIAN_POINT('Ctrl Pts',(-0.883802265143228,0.706216247449082,
9.52670835651243));
#10352=CARTESIAN_POINT('Ctrl Pts',(-1.12337158667086,0.127730392023871,
9.55209135669275));
#10353=CARTESIAN_POINT('Ctrl Pts',(-1.01848866350395,-0.489110854542463,
9.57745792779555));
#10354=CARTESIAN_POINT('Ctrl Pts',(-0.60179472455561,-0.955301301450795,
9.60280723074089));
#10355=CARTESIAN_POINT('Ctrl Pts',(-0.001370421070526,-1.12820692400817,
9.62813825936887));
#10356=CARTESIAN_POINT('Ctrl Pts',(0.598555103765798,-0.955298231036643,
9.65345008884992));
#10357=CARTESIAN_POINT('Ctrl Pts',(1.01419982916296,-0.490081317342479,
9.67874178759014));
#10358=CARTESIAN_POINT('Ctrl Pts',(1.11853453908254,0.124451303977719,9.70401243962266));
#10359=CARTESIAN_POINT('Ctrl Pts',(0.880130003500144,0.699796852270577,
9.72926114655504));
#10360=CARTESIAN_POINT('Ctrl Pts',(0.372621603087543,1.05978697679078,9.75448701500854));
#10361=CARTESIAN_POINT('Ctrl Pts',(-0.248041992658389,1.09455009643884,
9.77968916982561));
#10362=CARTESIAN_POINT('Ctrl Pts',(-0.791539658878634,0.79406385342954,
9.80486674471668));
#10363=CARTESIAN_POINT('Ctrl Pts',(-1.0915642463606,0.251016259244287,9.83001890502188));
#10364=CARTESIAN_POINT('Ctrl Pts',(-1.05672913961632,-0.367760770678466,
9.85514476310435));
#10365=CARTESIAN_POINT('Ctrl Pts',(-0.698424490262498,-0.872650684411287,
9.88024361655606));
#10366=CARTESIAN_POINT('Ctrl Pts',(-0.127087637559715,-1.10920064273684,
9.90531437209189));
#10367=CARTESIAN_POINT('Ctrl Pts',(0.481799407328479,-1.00580708103632,
9.93035686134745));
#10368=CARTESIAN_POINT('Ctrl Pts',(0.941725418794725,-0.59448291764376,
9.95536888870454));
#10369=CARTESIAN_POINT('Ctrl Pts',(1.05528916776323,-0.200207605714132,
9.97202614010278));
#10370=CARTESIAN_POINT('Ctrl Pts',(1.05531580562393,-0.00233479057547877,
9.98034674015783));
#10371=CARTESIAN_POINT('Ctrl Pts',(0.932817338094398,0.00223903224158551,
7.22153832457769));
#10372=CARTESIAN_POINT('Ctrl Pts',(0.932793760066264,0.177382610654345,
7.22890315462753));
#10373=CARTESIAN_POINT('Ctrl Pts',(0.832403451678301,0.525794592256776,
7.2436226723496));
#10374=CARTESIAN_POINT('Ctrl Pts',(0.425685989057847,0.889621198330929,
7.26574445281166));
#10375=CARTESIAN_POINT('Ctrl Pts',(-0.112909767544801,0.981053680306889,
7.28789420673005));
#10376=CARTESIAN_POINT('Ctrl Pts',(-0.618460222818951,0.771777784533472,
7.3100782388979));
#10377=CARTESIAN_POINT('Ctrl Pts',(-0.935649120831108,0.324866303046137,
7.33229486959658));
#10378=CARTESIAN_POINT('Ctrl Pts',(-0.966533418354376,-0.223107019260836,
7.35454598288692));
#10379=CARTESIAN_POINT('Ctrl Pts',(-0.700735671162198,-0.704290462461527,
7.37683185460622));
#10380=CARTESIAN_POINT('Ctrl Pts',(-0.218915760021475,-0.970728950195303,
7.39915346188169));
#10381=CARTESIAN_POINT('Ctrl Pts',(0.331698104933367,-0.93994104524836,
7.42151144978389));
#10382=CARTESIAN_POINT('Ctrl Pts',(0.782282737482763,-0.620400150468231,
7.44390658058016));
#10383=CARTESIAN_POINT('Ctrl Pts',(0.994149823047339,-0.109251837914898,
7.46633954009742));
#10384=CARTESIAN_POINT('Ctrl Pts',(0.90145062659539,0.437203917789278,7.48881101627259));
#10385=CARTESIAN_POINT('Ctrl Pts',(0.53155858950099,0.851305491311238,7.51132167468147));
#10386=CARTESIAN_POINT('Ctrl Pts',(-0.00283212755745073,1.00540470537402,
7.53387212978628));
#10387=CARTESIAN_POINT('Ctrl Pts',(-0.538394652874874,0.851310115270327,
7.55646305016228));
#10388=CARTESIAN_POINT('Ctrl Pts',(-0.896468296303925,0.450516088130438,
7.578256674521));
#10389=CARTESIAN_POINT('Ctrl Pts',(-0.998150334469993,-0.0528799063122484,
7.59924871335334));
#10390=CARTESIAN_POINT('Ctrl Pts',(-0.852714766181271,-0.524739769713425,
7.61943418917057));
#10391=CARTESIAN_POINT('Ctrl Pts',(-0.498767893239097,-0.870058344680294,
7.63965341026417));
#10392=CARTESIAN_POINT('Ctrl Pts',(-0.0217992891188254,-1.00474195617444,
7.65990693434088));
#10393=CARTESIAN_POINT('Ctrl Pts',(0.461590577887178,-0.893841791987376,
7.68019475056593));
#10394=CARTESIAN_POINT('Ctrl Pts',(0.897713484577771,-0.511087829973259,
7.70390421214106));
#10395=CARTESIAN_POINT('Ctrl Pts',(1.05284739986986,0.161816435506151,7.73105822118701));
#10396=CARTESIAN_POINT('Ctrl Pts',(0.705905536489394,0.760893081895744,
7.75828300274897));
#10397=CARTESIAN_POINT('Ctrl Pts',(0.172854320016419,1.00020564829781,7.78215786321883));
#10398=CARTESIAN_POINT('Ctrl Pts',(-0.326951940005122,0.96300872535927,
7.8026582555522));
#10399=CARTESIAN_POINT('Ctrl Pts',(-0.713843829504815,0.71294984730384,
7.821483056657));
#10400=CARTESIAN_POINT('Ctrl Pts',(-0.933658986576131,0.362739327222884,
7.83862346287265));
#10401=CARTESIAN_POINT('Ctrl Pts',(-1.00323184902305,-0.0035998581910392,
7.85407042530536));
#10402=CARTESIAN_POINT('Ctrl Pts',(-0.933551814627203,-0.369979955877476,
7.86953812136651));
#10403=CARTESIAN_POINT('Ctrl Pts',(-0.669479465575597,-0.793075720570871,
7.89018956759317));
#10404=CARTESIAN_POINT('Ctrl Pts',(-0.0780371137366919,-1.07927635268795,
7.9160552500025));
#10405=CARTESIAN_POINT('Ctrl Pts',(0.679227399735273,-0.846195851440705,
7.94717855408861));
#10406=CARTESIAN_POINT('Ctrl Pts',(1.0761201749552,-0.158934193380002,7.97838613962336));
#10407=CARTESIAN_POINT('Ctrl Pts',(0.899726434462559,0.617015767811971,
8.00967853755681));
#10408=CARTESIAN_POINT('Ctrl Pts',(0.239950968779785,1.06735347443573,8.04105594349517));
#10409=CARTESIAN_POINT('Ctrl Pts',(-0.462527249163799,0.96075330324454,
8.06902253694048));
#10410=CARTESIAN_POINT('Ctrl Pts',(-0.891570403389457,0.540551941686763,
8.09354880324681));
#10411=CARTESIAN_POINT('Ctrl Pts',(-1.04369474513434,0.0487982002092891,
8.1146091329916));
#10412=CARTESIAN_POINT('Ctrl Pts',(-0.9414272520629,-0.457221001910597,
8.13570732602349));
#10413=CARTESIAN_POINT('Ctrl Pts',(-0.609430038442986,-0.853524812483484,
8.15684347905607));
#10414=CARTESIAN_POINT('Ctrl Pts',(-0.247795399191627,-0.995191046143806,
8.17272380746048));
#10415=CARTESIAN_POINT('Ctrl Pts',(0.00354110646814628,-1.01069610287633,
8.18332260701429));
#10416=CARTESIAN_POINT('Ctrl Pts',(0.171091478472033,-1.00027000944185,
8.19039160004791));
#10417=CARTESIAN_POINT('Ctrl Pts',(0.417066703556737,-0.93784914346088,
8.20100213932378));
#10418=CARTESIAN_POINT('Ctrl Pts',(0.705699028395263,-0.755937475658024,
8.21516517881097));
#10419=CARTESIAN_POINT('Ctrl Pts',(1.01262165785068,-0.343507499055525,
8.2364379486868));
#10420=CARTESIAN_POINT('Ctrl Pts',(1.06497976343805,0.330755715265788,8.26308166354529));
#10421=CARTESIAN_POINT('Ctrl Pts',(0.555379063018134,0.969841090340963,
8.29513806421836));
#10422=CARTESIAN_POINT('Ctrl Pts',(-0.184420846152002,1.08048275305726,
8.32459966541254));
#10423=CARTESIAN_POINT('Ctrl Pts',(-0.764151013947635,0.759084830483624,
8.35144330977293));
#10424=CARTESIAN_POINT('Ctrl Pts',(-1.05294715618884,0.237271017126475,
8.37564898068673));
#10425=CARTESIAN_POINT('Ctrl Pts',(-1.01969845552176,-0.360514646878159,
8.39990064760307));
#10426=CARTESIAN_POINT('Ctrl Pts',(-0.736987911228233,-0.758079682683477,
8.41969861730935));
#10427=CARTESIAN_POINT('Ctrl Pts',(-0.350967168984493,-0.994049689726893,
8.43862194344341));
#10428=CARTESIAN_POINT('Ctrl Pts',(0.0398642534826699,-1.06322766096296,
8.45486200074116));
#10429=CARTESIAN_POINT('Ctrl Pts',(0.461201683510019,-0.949886899588757,
8.47293247966593));
#10430=CARTESIAN_POINT('Ctrl Pts',(0.777368325383777,-0.716895360721043,
8.48921554936968));
#10431=CARTESIAN_POINT('Ctrl Pts',(0.986544217957618,-0.383737196400418,
8.50551849992385));
#10432=CARTESIAN_POINT('Ctrl Pts',(1.07247833681818,0.0677150502151257,
8.52456124674014));
#10433=CARTESIAN_POINT('Ctrl Pts',(0.924204185518489,0.584244428195864,
8.54635705344648));
#10434=CARTESIAN_POINT('Ctrl Pts',(0.472384193043772,0.988084733067928,
8.57092035603831));
#10435=CARTESIAN_POINT('Ctrl Pts',(-0.125803338746724,1.08987257428914,
8.59552639540173));
#10436=CARTESIAN_POINT('Ctrl Pts',(-0.687539065826917,0.857373679191502,
8.62017455944292));
#10437=CARTESIAN_POINT('Ctrl Pts',(-1.04001445832212,0.360821877226519,
8.64486434049305));
#10438=CARTESIAN_POINT('Ctrl Pts',(-1.07436123594458,-0.24816575006392,
8.66959514941773));
#10439=CARTESIAN_POINT('Ctrl Pts',(-0.778947264478789,-0.782953832069739,
8.69436639905966));
#10440=CARTESIAN_POINT('Ctrl Pts',(-0.243432346581132,-1.07907670088945,
8.71917746747984));
#10441=CARTESIAN_POINT('Ctrl Pts',(0.368514215010823,-1.04484341046501,
8.74402771279146));
#10442=CARTESIAN_POINT('Ctrl Pts',(0.869226914069874,-0.68973145530312,
8.76891647464699));
#10443=CARTESIAN_POINT('Ctrl Pts',(1.10461409169443,-0.121791671725091,
8.79384306738233));
#10444=CARTESIAN_POINT('Ctrl Pts',(1.00161987568289,0.485230960329545,8.8188067900524));
#10445=CARTESIAN_POINT('Ctrl Pts',(0.590837878571582,0.945084633471956,
8.84380691007165));
#10446=CARTESIAN_POINT('Ctrl Pts',(-0.00241534456593945,1.11614188043567,
8.86884270930869));
#10447=CARTESIAN_POINT('Ctrl Pts',(-0.596684097120054,0.945119650310722,
8.89391338364207));
#10448=CARTESIAN_POINT('Ctrl Pts',(-0.993843243593392,0.500590727563871,
8.91808845535031));
#10449=CARTESIAN_POINT('Ctrl Pts',(-1.10643245721144,-0.0575015772983971,
8.94136267937612));
#10450=CARTESIAN_POINT('Ctrl Pts',(-0.945619796602633,-0.580262658763286,
8.96373116543371));
#10451=CARTESIAN_POINT('Ctrl Pts',(-0.586107215046292,-0.93104338567574,
8.98425885454782));
#10452=CARTESIAN_POINT('Ctrl Pts',(-0.160798094550997,-1.07909003162016,
9.00293848626054));
#10453=CARTESIAN_POINT('Ctrl Pts',(0.380847821757762,-1.06040707411611,
9.02537151954004));
#10454=CARTESIAN_POINT('Ctrl Pts',(0.85238767414114,-0.740715209958907,
9.04783210789513));
#10455=CARTESIAN_POINT('Ctrl Pts',(1.06757064773678,-0.241674799716118,
9.07031749990356));
#10456=CARTESIAN_POINT('Ctrl Pts',(1.08989480948035,0.30055574321441,9.09281927275907));
#10457=CARTESIAN_POINT('Ctrl Pts',(0.732714846524938,0.921690446594372,
9.12097849776537));
#10458=CARTESIAN_POINT('Ctrl Pts',(0.0475037480025504,1.13202296039076,
9.14917647651982));
#10459=CARTESIAN_POINT('Ctrl Pts',(-0.47863811734372,0.989412084764905,
9.17175595217751));
#10460=CARTESIAN_POINT('Ctrl Pts',(-0.844340163433761,0.720354496408093,
9.19058402886265));
#10461=CARTESIAN_POINT('Ctrl Pts',(-1.08711624461903,0.275017683314028,
9.21131102491027));
#10462=CARTESIAN_POINT('Ctrl Pts',(-1.08678177842939,-0.278315106506191,
9.23393881798215));
#10463=CARTESIAN_POINT('Ctrl Pts',(-0.822280508726689,-0.765009547413839,
9.25658444333911));
#10464=CARTESIAN_POINT('Ctrl Pts',(-0.356463083692494,-1.06542928247866,
9.27924670945844));
#10465=CARTESIAN_POINT('Ctrl Pts',(0.196587215171616,-1.10729173992762,
9.30192398401361));
#10466=CARTESIAN_POINT('Ctrl Pts',(0.581247622139915,-0.933498715306414,
9.31918146203166));
#10467=CARTESIAN_POINT('Ctrl Pts',(0.78805035283314,-0.743174183407583,
9.33100500669254));
#10468=CARTESIAN_POINT('Ctrl Pts',(0.916397144732695,-0.586774635437394,
9.339519544202));
#10469=CARTESIAN_POINT('Ctrl Pts',(1.08075456481652,-0.269770476008509,
9.35442396179574));
#10470=CARTESIAN_POINT('Ctrl Pts',(1.1043406223813,0.149554271447882,9.37146787576897));
#10471=CARTESIAN_POINT('Ctrl Pts',(0.958119700633825,0.530862407294559,
9.38851799488734));
#10472=CARTESIAN_POINT('Ctrl Pts',(0.713059280154455,0.857531088386705,
9.4055734547437));
#10473=CARTESIAN_POINT('Ctrl Pts',(0.252911145537254,1.11223884436659,9.42690335124296));
#10474=CARTESIAN_POINT('Ctrl Pts',(-0.377817110739569,1.07678655749214,
9.45251244753617));
#10475=CARTESIAN_POINT('Ctrl Pts',(-0.893151735400408,0.711201885990653,
9.47813454118543));
#10476=CARTESIAN_POINT('Ctrl Pts',(-1.13514464160495,0.12712014183053,9.50376820319782));
#10477=CARTESIAN_POINT('Ctrl Pts',(-1.0292241515188,-0.496405026542247,
9.52941250474413));
#10478=CARTESIAN_POINT('Ctrl Pts',(-0.607651992297783,-0.968196730147786,
9.55506626992792));
#10479=CARTESIAN_POINT('Ctrl Pts',(0.000516788824355856,-1.14343121492963,
9.58072843587768));
#10480=CARTESIAN_POINT('Ctrl Pts',(0.608868148912967,-0.968192123375259,
9.60639786060031));
#10481=CARTESIAN_POINT('Ctrl Pts',(1.03084013393238,-0.496034157006386,
9.63207344185143));
#10482=CARTESIAN_POINT('Ctrl Pts',(1.13694700570821,0.128377444332003,9.6577540442593));
#10483=CARTESIAN_POINT('Ctrl Pts',(0.894542209160189,0.713620555570391,
9.68343855267843));
#10484=CARTESIAN_POINT('Ctrl Pts',(0.377864659011472,1.08022831008716,9.70912582606619));
#10485=CARTESIAN_POINT('Ctrl Pts',(-0.254708500473694,1.11575062973695,
9.73481475003169));
#10486=CARTESIAN_POINT('Ctrl Pts',(-0.809235469376882,0.809269589714066,
9.76050416245622));
#10487=CARTESIAN_POINT('Ctrl Pts',(-1.11570364867539,0.254741293244564,
9.78619302028867));
#10488=CARTESIAN_POINT('Ctrl Pts',(-1.08017949873475,-0.377791903239077,
9.81187998879018));
#10489=CARTESIAN_POINT('Ctrl Pts',(-0.71362254477927,-0.894447905725997,
9.83756442934909));
#10490=CARTESIAN_POINT('Ctrl Pts',(-0.12848878406753,-1.13680446508768,
9.86324414525839));
#10491=CARTESIAN_POINT('Ctrl Pts',(0.495751120741053,-1.03087493259538,
9.88892046721288));
#10492=CARTESIAN_POINT('Ctrl Pts',(0.967762675373715,-0.608896178670159,
9.91458687730015));
#10493=CARTESIAN_POINT('Ctrl Pts',(1.08449349913632,-0.20388861139028,9.93170092751877));
#10494=CARTESIAN_POINT('Ctrl Pts',(1.08452085900721,-0.000652520652106218,
9.94024705461864));
#10495=CARTESIAN_POINT('Ctrl Pts',(0.916384184646393,-0.000812414047608488,
7.294052389051));
#10496=CARTESIAN_POINT('Ctrl Pts',(0.91636102789669,0.171201801238968,7.30128562862064));
#10497=CARTESIAN_POINT('Ctrl Pts',(0.817714321229081,0.513121139438122,
7.31573445825018));
#10498=CARTESIAN_POINT('Ctrl Pts',(0.419183940001587,0.869421294661586,
7.33740687562125));
#10499=CARTESIAN_POINT('Ctrl Pts',(-0.107511678749076,0.958699494084228,
7.35906851046912));
#10500=CARTESIAN_POINT('Ctrl Pts',(-0.600919896114351,0.754308982034972,
7.38072396635307));
#10501=CARTESIAN_POINT('Ctrl Pts',(-0.90986434389333,0.318796907723617,
7.40237277329793));
#10502=CARTESIAN_POINT('Ctrl Pts',(-0.939775508284088,-0.214171715938281,
7.42401675026896));
#10503=CARTESIAN_POINT('Ctrl Pts',(-0.681599841371247,-0.681292688788261,
7.44565670173072));
#10504=CARTESIAN_POINT('Ctrl Pts',(-0.214544410932947,-0.939420652432807,
7.46729389336328));
#10505=CARTESIAN_POINT('Ctrl Pts',(0.318210121393327,-0.909504154003217,
7.48892939490667));
#10506=CARTESIAN_POINT('Ctrl Pts',(0.753380323755671,-0.600740800554072,
7.51056436224741));
#10507=CARTESIAN_POINT('Ctrl Pts',(0.957580132215121,-0.107767532236841,
7.53219991215366));
#10508=CARTESIAN_POINT('Ctrl Pts',(0.868211541183081,0.418326077149899,
7.55383719616653));
#10509=CARTESIAN_POINT('Ctrl Pts',(0.512571933875558,0.816291655068875,
7.5754773236975));
#10510=CARTESIAN_POINT('Ctrl Pts',(-0.000319842256805562,0.964068440570839,
7.59712147475655));
#10511=CARTESIAN_POINT('Ctrl Pts',(-0.513473050755741,0.816299802289933,
7.61877069085977));
#10512=CARTESIAN_POINT('Ctrl Pts',(-0.855981669773446,0.432764156671664,
7.63962426478969));
#10513=CARTESIAN_POINT('Ctrl Pts',(-0.953048966078777,-0.0481973160739187,
7.65968184621655));
#10514=CARTESIAN_POINT('Ctrl Pts',(-0.814207366238296,-0.498404503042273,
7.67894394873332));
#10515=CARTESIAN_POINT('Ctrl Pts',(-0.476868785727358,-0.827423916195667,
7.69821324881017));
#10516=CARTESIAN_POINT('Ctrl Pts',(-0.0229026114670843,-0.955530455908849,
7.71749025791405));
#10517=CARTESIAN_POINT('Ctrl Pts',(0.436569596441587,-0.85005354508792,
7.73677624340631));
#10518=CARTESIAN_POINT('Ctrl Pts',(0.850579801372237,-0.486583791265893,
7.75928808298809));
#10519=CARTESIAN_POINT('Ctrl Pts',(0.997455702178448,0.151411719541167,
7.7850346645544));
#10520=CARTESIAN_POINT('Ctrl Pts',(0.66892061877028,0.718298327157484,7.81080466018562));
#10521=CARTESIAN_POINT('Ctrl Pts',(0.165105277263114,0.944401326593409,
7.83337036699914));
#10522=CARTESIAN_POINT('Ctrl Pts',(-0.306760321133552,0.909226016129731,
7.85272560376473));
#10523=CARTESIAN_POINT('Ctrl Pts',(-0.671629161971406,0.673332022752352,
7.87048190618396));
#10524=CARTESIAN_POINT('Ctrl Pts',(-0.878741185245582,0.343312833427155,
7.88663430695027));
#10525=CARTESIAN_POINT('Ctrl Pts',(-0.94423011831239,-0.00164456370475496,
7.90118025371029));
#10526=CARTESIAN_POINT('Ctrl Pts',(-0.878646080781751,-0.346381218378189,
7.91573520582742));
#10527=CARTESIAN_POINT('Ctrl Pts',(-0.630315057219919,-0.74419509882429,
7.93515396976183));
#10528=CARTESIAN_POINT('Ctrl Pts',(-0.0746840041171197,-1.01290792724034,
7.95945317547552));
#10529=CARTESIAN_POINT('Ctrl Pts',(0.635655594458093,-0.79408428312529,
7.98865203565831));
#10530=CARTESIAN_POINT('Ctrl Pts',(1.00738408651088,-0.150077117453577,
8.01789434930099));
#10531=CARTESIAN_POINT('Ctrl Pts',(0.842150637204844,0.576077696538741,
8.04718205840345));
#10532=CARTESIAN_POINT('Ctrl Pts',(0.225271464949242,0.996955646093593,
8.07651744286865));
#10533=CARTESIAN_POINT('Ctrl Pts',(-0.43077106632299,0.897282204130466,
8.10263821657078));
#10534=CARTESIAN_POINT('Ctrl Pts',(-0.831114549612531,0.505125213112986,
8.12552681825321));
#10535=CARTESIAN_POINT('Ctrl Pts',(-0.972961487683506,0.0464809015971219,
8.14516966456063));
#10536=CARTESIAN_POINT('Ctrl Pts',(-0.877602512982472,-0.425191958105245,
8.16483693107729));
#10537=CARTESIAN_POINT('Ctrl Pts',(-0.568276019795686,-0.794384958085934,
8.18452868985693));
#10538=CARTESIAN_POINT('Ctrl Pts',(-0.231513901591766,-0.926289452386036,
8.19931732873309));
#10539=CARTESIAN_POINT('Ctrl Pts',(0.00245799136279632,-0.940722053136144,
8.20918392331538));
#10540=CARTESIAN_POINT('Ctrl Pts',(0.158416318109175,-0.931017174660892,
8.21576392644465));
#10541=CARTESIAN_POINT('Ctrl Pts',(0.387337229899669,-0.872920481534924,
8.22563902104255));
#10542=CARTESIAN_POINT('Ctrl Pts',(0.655887282970169,-0.703657924089153,
8.23881727887628));
#10543=CARTESIAN_POINT('Ctrl Pts',(0.941363930700124,-0.320023744551051,
8.25860467543646));
#10544=CARTESIAN_POINT('Ctrl Pts',(0.98998838540909,0.306890866588042,8.28337764757458));
#10545=CARTESIAN_POINT('Ctrl Pts',(0.516353784183733,0.900777750505931,
8.31317026550616));
#10546=CARTESIAN_POINT('Ctrl Pts',(-0.170895376698677,1.00351776465295,
8.34053992286506));
#10547=CARTESIAN_POINT('Ctrl Pts',(-0.709276893706946,0.705023452750632,
8.36547008485353));
#10548=CARTESIAN_POINT('Ctrl Pts',(-0.977416665651329,0.220507453202623,
8.38794586803964));
#10549=CARTESIAN_POINT('Ctrl Pts',(-0.946540072103369,-0.334455386118879,
8.41046071721602));
#10550=CARTESIAN_POINT('Ctrl Pts',(-0.68410690604905,-0.703498657680165,
8.42883889692179));
#10551=CARTESIAN_POINT('Ctrl Pts',(-0.325798798725742,-0.922527998573711,
8.44640383700852));
#10552=CARTESIAN_POINT('Ctrl Pts',(0.0369623652280897,-0.986736749875426,
8.46147757987718));
#10553=CARTESIAN_POINT('Ctrl Pts',(0.428035342802407,-0.881538480517849,
8.47825020517938));
#10554=CARTESIAN_POINT('Ctrl Pts',(0.721493797857177,-0.665282361395511,
8.49336377211604));
#10555=CARTESIAN_POINT('Ctrl Pts',(0.915653860248132,-0.356045284728461,
8.50849631732876));
#10556=CARTESIAN_POINT('Ctrl Pts',(0.995424601695212,0.0630116385503096,
8.52617266101546));
#10557=CARTESIAN_POINT('Ctrl Pts',(0.857789064698206,0.542518419007572,
8.54640619473492));
#10558=CARTESIAN_POINT('Ctrl Pts',(0.438308728778306,0.917473083752972,
8.56921188084219));
#10559=CARTESIAN_POINT('Ctrl Pts',(-0.117171435160921,1.01201202635041,
8.59206127082509));
#10560=CARTESIAN_POINT('Ctrl Pts',(-0.638927134962905,0.79608335109431,
8.61495471428855));
#10561=CARTESIAN_POINT('Ctrl Pts',(-0.966415516773689,0.334773910945176,
8.63789269515097));
#10562=CARTESIAN_POINT('Ctrl Pts',(-0.99836233251678,-0.231176077678445,
8.66087559759738));
#10563=CARTESIAN_POINT('Ctrl Pts',(-0.723758542776752,-0.72835451264945,
8.68390381202748));
#10564=CARTESIAN_POINT('Ctrl Pts',(-0.2257474509395,-1.00377738419217,8.70697768864429));
#10565=CARTESIAN_POINT('Ctrl Pts',(0.343600136828314,-0.971963977022025,
8.73009755919227));
#10566=CARTESIAN_POINT('Ctrl Pts',(0.809690300867129,-0.641455706076566,
8.75326372412054));
#10567=CARTESIAN_POINT('Ctrl Pts',(1.02893814149207,-0.112569327400558,
8.77647646087813));
#10568=CARTESIAN_POINT('Ctrl Pts',(0.933018095440899,0.453037359706394,
8.79973601914518));
#10569=CARTESIAN_POINT('Ctrl Pts',(0.550088474279159,0.881786204706492,
8.82304262430822));
#10570=CARTESIAN_POINT('Ctrl Pts',(-0.00331223803182207,1.04140779084441,
8.84639646939416));
#10571=CARTESIAN_POINT('Ctrl Pts',(-0.558044053109453,0.881822628119523,
8.86979773274531));
#10572=CARTESIAN_POINT('Ctrl Pts',(-0.929061567856926,0.46663875567079,
8.89237806561174));
#10573=CARTESIAN_POINT('Ctrl Pts',(-1.03434228395829,-0.0550007789708017,
8.91413164432233));
#10574=CARTESIAN_POINT('Ctrl Pts',(-0.883973293660551,-0.543961856211894,
8.93505289544298));
#10575=CARTESIAN_POINT('Ctrl Pts',(-0.547515238324857,-0.872307713095914,
8.95426532130326));
#10576=CARTESIAN_POINT('Ctrl Pts',(-0.149203363966445,-1.01097948256328,
8.97175868300262));
#10577=CARTESIAN_POINT('Ctrl Pts',(0.358343864201227,-0.993501252395768,
8.99277925477119));
#10578=CARTESIAN_POINT('Ctrl Pts',(0.800624893951803,-0.693778031940356,
9.01384209964755));
#10579=CARTESIAN_POINT('Ctrl Pts',(1.00264542737942,-0.225346188642404,
9.03494770829309));
#10580=CARTESIAN_POINT('Ctrl Pts',(1.02364288737243,0.283933103839578,9.05608172922299));
#10581=CARTESIAN_POINT('Ctrl Pts',(0.688000806473435,0.867935649292769,
9.08255185043447));
#10582=CARTESIAN_POINT('Ctrl Pts',(0.0430534476606014,1.06608732574115,
9.10909256714991));
#10583=CARTESIAN_POINT('Ctrl Pts',(-0.452738363714565,0.93174161838465,
9.13036778259929));
#10584=CARTESIAN_POINT('Ctrl Pts',(-0.797580117742964,0.678064020635429,
9.14812059831063));
#10585=CARTESIAN_POINT('Ctrl Pts',(-1.02673710165334,0.257847579606903,
9.16767814991022));
#10586=CARTESIAN_POINT('Ctrl Pts',(-1.02648106844828,-0.264826941713865,
9.18905154450334));
#10587=CARTESIAN_POINT('Ctrl Pts',(-0.776460073134754,-0.725026353915674,
9.21046173226614));
#10588=CARTESIAN_POINT('Ctrl Pts',(-0.33562848698493,-1.00940897138283,
9.23190879544451));
#10589=CARTESIAN_POINT('Ctrl Pts',(0.188329899581691,-1.0491402456296,9.25339297598941));
#10590=CARTESIAN_POINT('Ctrl Pts',(0.553136534120908,-0.884368968829443,
9.26975676409425));
#10591=CARTESIAN_POINT('Ctrl Pts',(0.749404683996913,-0.703743773738387,
9.28097769251118));
#10592=CARTESIAN_POINT('Ctrl Pts',(0.871248898640151,-0.555270911284687,
9.28906053551857));
#10593=CARTESIAN_POINT('Ctrl Pts',(1.02735904501533,-0.254207860668812,
9.30321546934299));
#10594=CARTESIAN_POINT('Ctrl Pts',(1.04984503084766,0.144376165230818,9.31941439398456));
#10595=CARTESIAN_POINT('Ctrl Pts',(0.910732980180467,0.507198490051187,
9.33563696536372));
#10596=CARTESIAN_POINT('Ctrl Pts',(0.677430691215826,0.818220810897905,
9.3518744741977));
#10597=CARTESIAN_POINT('Ctrl Pts',(0.238978705298457,1.0610211403517,9.37219870850224));
#10598=CARTESIAN_POINT('Ctrl Pts',(-0.362859301163257,1.02730471082093,
9.39663266712745));
#10599=CARTESIAN_POINT('Ctrl Pts',(-0.855287575123984,0.678104309011124,
9.42111055993154));
#10600=CARTESIAN_POINT('Ctrl Pts',(-1.08690633568849,0.119360359866055,
9.44563212936705));
#10601=CARTESIAN_POINT('Ctrl Pts',(-0.98555083882038,-0.47798510234353,
9.47019679120956));
#10602=CARTESIAN_POINT('Ctrl Pts',(-0.581229979579629,-0.930648430527953,
9.49480407397801));
#10603=CARTESIAN_POINT('Ctrl Pts',(0.00295283093870749,-1.09909733418053,
9.51945343242555));
#10604=CARTESIAN_POINT('Ctrl Pts',(0.588197155365154,-0.930641683598714,
9.54414431358483));
#10605=CARTESIAN_POINT('Ctrl Pts',(0.994786308140254,-0.475881984543007,
9.56887614236257));
#10606=CARTESIAN_POINT('Ctrl Pts',(1.09727215135844,0.126473271551238,9.59364831685043));
#10607=CARTESIAN_POINT('Ctrl Pts',(0.863198931394216,0.691932043003254,
9.61846022152596));
#10608=CARTESIAN_POINT('Ctrl Pts',(0.363371458512755,1.04674092501543,9.64331120732547));
#10609=CARTESIAN_POINT('Ctrl Pts',(-0.249563746611437,1.08129056426141,
9.66820062239446));
#10610=CARTESIAN_POINT('Ctrl Pts',(-0.787750701358366,0.78399163290601,
9.69312775992718));
#10611=CARTESIAN_POINT('Ctrl Pts',(-1.0857205254415,0.245119969922457,9.71809198124987));
#10612=CARTESIAN_POINT('Ctrl Pts',(-1.05128010206474,-0.370570820675122,
9.74309241562914));
#10613=CARTESIAN_POINT('Ctrl Pts',(-0.694056959651085,-0.874314390372112,
9.76812867801744));
#10614=CARTESIAN_POINT('Ctrl Pts',(-0.122812930922393,-1.11106608042246,
9.79319923890406));
#10615=CARTESIAN_POINT('Ctrl Pts',(0.487625669319352,-1.007614700358,9.81830510245824));
#10616=CARTESIAN_POINT('Ctrl Pts',(0.950000744760197,-0.594415484013305,
9.84344158104869));
#10617=CARTESIAN_POINT('Ctrl Pts',(1.06455322262812,-0.197156271448973,
9.86022677005009));
#10618=CARTESIAN_POINT('Ctrl Pts',(1.06458008203471,0.00236224302569044,
9.86861657216291));
#10619=CARTESIAN_POINT('Ctrl Pts',(0.962718230280815,-0.00325963339072736,
7.35239823212382));
#10620=CARTESIAN_POINT('Ctrl Pts',(0.96269391832364,0.177335756254699,7.35999231216134));
#10621=CARTESIAN_POINT('Ctrl Pts',(0.859091395002888,0.536367440659574,
7.37516300480678));
#10622=CARTESIAN_POINT('Ctrl Pts',(0.441244001169262,0.909763722620838,
7.39787937610872));
#10623=CARTESIAN_POINT('Ctrl Pts',(-0.110083694811868,1.0031262480341,7.42055272981597));
#10624=CARTESIAN_POINT('Ctrl Pts',(-0.625739413289849,0.789385321248754,
7.44318475760545));
#10625=CARTESIAN_POINT('Ctrl Pts',(-0.94804788351903,0.334822437451381,
7.46577552364345));
#10626=CARTESIAN_POINT('Ctrl Pts',(-0.979088619717144,-0.220522420853946,
7.48832585783457));
#10627=CARTESIAN_POINT('Ctrl Pts',(-0.710391608174497,-0.706415596651747,
7.51083627889516));
#10628=CARTESIAN_POINT('Ctrl Pts',(-0.225225071456474,-0.97440720732087,
7.53330747523763));
#10629=CARTESIAN_POINT('Ctrl Pts',(0.327204367923681,-0.943256814728376,
7.55574009450392));
#10630=CARTESIAN_POINT('Ctrl Pts',(0.777625996912355,-0.623512949022436,
7.57813482755551));
#10631=CARTESIAN_POINT('Ctrl Pts',(0.988540004465044,-0.113987597368397,
7.60049237934514));
#10632=CARTESIAN_POINT('Ctrl Pts',(0.896206941446668,0.4287655787072,7.62281347470688));
#10633=CARTESIAN_POINT('Ctrl Pts',(0.529825699099087,0.838550426236005,
7.64509886891068));
#10634=CARTESIAN_POINT('Ctrl Pts',(0.00247375335561738,0.990354343679899,
7.66734929755787));
#10635=CARTESIAN_POINT('Ctrl Pts',(-0.524138115921198,0.838567973237236,
7.68956560662869));
#10636=CARTESIAN_POINT('Ctrl Pts',(-0.874927095876008,0.44556549648226,
7.71092685158314));
#10637=CARTESIAN_POINT('Ctrl Pts',(-0.974100408150317,-0.0463432791829163,
7.73143835597165));
#10638=CARTESIAN_POINT('Ctrl Pts',(-0.832242715660948,-0.506006054432365,
7.75110411184544));
#10639=CARTESIAN_POINT('Ctrl Pts',(-0.488286707768319,-0.841336359336464,
7.77074553879654));
#10640=CARTESIAN_POINT('Ctrl Pts',(-0.0262305298762631,-0.971625611540388,
7.79036342458605));
#10641=CARTESIAN_POINT('Ctrl Pts',(0.440601778900192,-0.864355709837979,
7.80995806390901));
#10642=CARTESIAN_POINT('Ctrl Pts',(0.860506937013534,-0.495559957146942,
7.83279185554976));
#10643=CARTESIAN_POINT('Ctrl Pts',(1.00887636243662,0.150329159697506,7.8588498166984));
#10644=CARTESIAN_POINT('Ctrl Pts',(0.676895321423857,0.722550287249622,
7.88486552355294));
#10645=CARTESIAN_POINT('Ctrl Pts',(0.169196097474721,0.950263594233254,
7.90760172054666));
#10646=CARTESIAN_POINT('Ctrl Pts',(-0.305463577404435,0.914780507645835,
7.9270708861676));
#10647=CARTESIAN_POINT('Ctrl Pts',(-0.671810169761784,0.677822910309403,
7.94489953704969));
#10648=CARTESIAN_POINT('Ctrl Pts',(-0.879447912476032,0.346878272400615,
7.96109498578419));
#10649=CARTESIAN_POINT('Ctrl Pts',(-0.944987627577209,0.00140801812198339,
7.97566103547143));
#10650=CARTESIAN_POINT('Ctrl Pts',(-0.879352813477502,-0.343383692137119,
7.99021763892266));
#10651=CARTESIAN_POINT('Ctrl Pts',(-0.631225667469588,-0.740751352130975,
8.00961452012653));
#10652=CARTESIAN_POINT('Ctrl Pts',(-0.0771397493560771,-1.00839347936742,
8.03383644726459));
#10653=CARTESIAN_POINT('Ctrl Pts',(0.629177191130674,-0.790429234820235,
8.06287098714952));
#10654=CARTESIAN_POINT('Ctrl Pts',(0.997610200365256,-0.151417910261682,
8.09187470557712));
#10655=CARTESIAN_POINT('Ctrl Pts',(0.833777198875691,0.56702235109786,8.12085049620515));
#10656=CARTESIAN_POINT('Ctrl Pts',(0.224721714435626,0.982134093303416,
8.14980096634948));
#10657=CARTESIAN_POINT('Ctrl Pts',(-0.421115897262969,0.883719661262009,
8.17551361664085));
#10658=CARTESIAN_POINT('Ctrl Pts',(-0.814372361173212,0.498341989081361,
8.19800033305438));
#10659=CARTESIAN_POINT('Ctrl Pts',(-0.953427319669304,0.0484314344791073,
8.21726600639097));
#10660=CARTESIAN_POINT('Ctrl Pts',(-0.859948384303787,-0.413455741489949,
8.23652418724655));
#10661=CARTESIAN_POINT('Ctrl Pts',(-0.557437339114465,-0.774372047655641,
8.25577651913894));
#10662=CARTESIAN_POINT('Ctrl Pts',(-0.228690647482073,-0.903055243520952,
8.27021029594821));
#10663=CARTESIAN_POINT('Ctrl Pts',(-0.000515736396863631,-0.917128271832189,
8.27983239822654));
#10664=CARTESIAN_POINT('Ctrl Pts',(0.151517914219297,-0.907666032608045,
8.28624658587932));
#10665=CARTESIAN_POINT('Ctrl Pts',(0.374537923474286,-0.851052981986712,
8.29586674787202));
#10666=CARTESIAN_POINT('Ctrl Pts',(0.635885574200474,-0.686297071615076,
8.30869123230048));
#10667=CARTESIAN_POINT('Ctrl Pts',(0.913362706304005,-0.31330570504482,
8.32792585459235));
#10668=CARTESIAN_POINT('Ctrl Pts',(0.960298111398029,0.295105768078741,
8.35196483325124));
#10669=CARTESIAN_POINT('Ctrl Pts',(0.501465375120066,0.869873888531251,
8.38080476513217));
#10670=CARTESIAN_POINT('Ctrl Pts',(-0.162449147078619,0.968850911622415,
8.40724050705978));
#10671=CARTESIAN_POINT('Ctrl Pts',(-0.681456260321231,0.680932154126198,
8.43127468009259));
#10672=CARTESIAN_POINT('Ctrl Pts',(-0.939460097390127,0.214496687258891,
8.45290679063804));
#10673=CARTESIAN_POINT('Ctrl Pts',(-0.909663908454563,-0.318827476974102,
8.47454207053821));
#10674=CARTESIAN_POINT('Ctrl Pts',(-0.657794745513012,-0.672857183575831,
8.49217320723589));
#10675=CARTESIAN_POINT('Ctrl Pts',(-0.314367073536956,-0.882767599732077,
8.50900742283414));
#10676=CARTESIAN_POINT('Ctrl Pts',(0.0329724123550007,-0.944188244476581,
8.52343929983286));
#10677=CARTESIAN_POINT('Ctrl Pts',(0.406941645978025,-0.843550008334516,
8.53947768998332));
#10678=CARTESIAN_POINT('Ctrl Pts',(0.687288910638273,-0.636918632610979,
8.55391643183634));
#10679=CARTESIAN_POINT('Ctrl Pts',(0.872566467708324,-0.341764473236915,
8.56835770756406));
#10680=CARTESIAN_POINT('Ctrl Pts',(0.948591468806281,0.0578163985634961,
8.58521127785539));
#10681=CARTESIAN_POINT('Ctrl Pts',(0.817421234004075,0.514441347046019,
8.60447819513267));
#10682=CARTESIAN_POINT('Ctrl Pts',(0.418417535373532,0.870947360259675,
8.62616498275342));
#10683=CARTESIAN_POINT('Ctrl Pts',(-0.109148101016243,0.960627692910106,
8.64786339052937));
#10684=CARTESIAN_POINT('Ctrl Pts',(-0.603968507622487,0.755735717138706,
8.66957489683606));
#10685=CARTESIAN_POINT('Ctrl Pts',(-0.914090995977477,0.318717601643026,
8.69130039086325));
#10686=CARTESIAN_POINT('Ctrl Pts',(-0.944218013863038,-0.216688417589151,
8.7130410220435));
#10687=CARTESIAN_POINT('Ctrl Pts',(-0.68467496995104,-0.686407268559419,
8.73479781719363));
#10688=CARTESIAN_POINT('Ctrl Pts',(-0.214641641910551,-0.946254378190861,
8.75657184998439));
#10689=CARTESIAN_POINT('Ctrl Pts',(0.322046159483052,-0.916178478730096,
8.77836416626867));
#10690=CARTESIAN_POINT('Ctrl Pts',(0.760864759580575,-0.60490496580893,
8.80017580379087));
#10691=CARTESIAN_POINT('Ctrl Pts',(0.967009403930397,-0.107413789658448,
8.8220077929034));
#10692=CARTESIAN_POINT('Ctrl Pts',(0.876805004086599,0.424019495378302,
8.84386114484036));
#10693=CARTESIAN_POINT('Ctrl Pts',(0.517305794945177,0.826421245036036,
8.86573687513684));
#10694=CARTESIAN_POINT('Ctrl Pts',(-0.00167454613960216,0.9760401976625,
8.8876359334133));
#10695=CARTESIAN_POINT('Ctrl Pts',(-0.521385932264157,0.826457735334773,
8.9095593580425));
#10696=CARTESIAN_POINT('Ctrl Pts',(-0.868640455956031,0.43777148600058,
8.93069501819422));
#10697=CARTESIAN_POINT('Ctrl Pts',(-0.967067305884696,-0.0501482616685878,
8.95104098324805));
#10698=CARTESIAN_POINT('Ctrl Pts',(-0.82647974711531,-0.507164794805139,
8.97059532406617));
#10699=CARTESIAN_POINT('Ctrl Pts',(-0.5121841740472,-0.813829042722063,
8.98854003426641));
#10700=CARTESIAN_POINT('Ctrl Pts',(-0.140348873654308,-0.943265643944857,
9.00486969124519));
#10701=CARTESIAN_POINT('Ctrl Pts',(0.333244783959833,-0.926930320777186,
9.02448345024546));
#10702=CARTESIAN_POINT('Ctrl Pts',(0.7456134311321,-0.6473862729714,9.04412252713801));
#10703=CARTESIAN_POINT('Ctrl Pts',(0.933852231346841,-0.210851073850686,
9.06379015343548));
#10704=CARTESIAN_POINT('Ctrl Pts',(0.953394997791234,0.263570308883686,
9.08347689733712));
#10705=CARTESIAN_POINT('Ctrl Pts',(0.640831730089639,0.807240118677375,
9.10811933138053));
#10706=CARTESIAN_POINT('Ctrl Pts',(0.0407574010195053,0.991527955790331,
9.13281136872211));
#10707=CARTESIAN_POINT('Ctrl Pts',(-0.420321639507707,0.866574252716919,
9.15259677633439));
#10708=CARTESIAN_POINT('Ctrl Pts',(-0.740930835144724,0.630710272872244,
9.16910201499638));
#10709=CARTESIAN_POINT('Ctrl Pts',(-0.953906223882338,0.240129411046737,
9.18727911280356));
#10710=CARTESIAN_POINT('Ctrl Pts',(-0.953649235823561,-0.245530083594935,
9.20713863170929));
#10711=CARTESIAN_POINT('Ctrl Pts',(-0.721385076575375,-0.673014021182606,
9.22702670918586));
#10712=CARTESIAN_POINT('Ctrl Pts',(-0.311975189904776,-0.937107659022901,
9.24694424499692));
#10713=CARTESIAN_POINT('Ctrl Pts',(0.174531516569616,-0.973987841354782,
9.26689261090667));
#10714=CARTESIAN_POINT('Ctrl Pts',(0.513193794898759,-0.821012780675783,
9.2820833145985));
#10715=CARTESIAN_POINT('Ctrl Pts',(0.695385853961652,-0.653341121506572,
9.29249948482213));
#10716=CARTESIAN_POINT('Ctrl Pts',(0.808487412662864,-0.515520951601559,
9.3000023335951));
#10717=CARTESIAN_POINT('Ctrl Pts',(0.953387192260482,-0.236072454603558,
9.31314087645884));
#10718=CARTESIAN_POINT('Ctrl Pts',(0.974249964060649,0.133859198164401,
9.32817495318504));
#10719=CARTESIAN_POINT('Ctrl Pts',(0.845142220453277,0.470585978846416,
9.34323069547589));
#10720=CARTESIAN_POINT('Ctrl Pts',(0.628623531777474,0.759231089356386,
9.35829990911351));
#10721=CARTESIAN_POINT('Ctrl Pts',(0.221724378384738,0.984555659606961,
9.37716126766761));
#10722=CARTESIAN_POINT('Ctrl Pts',(-0.336811565884306,0.953266271395749,
9.39983708161437));
#10723=CARTESIAN_POINT('Ctrl Pts',(-0.793838921575871,0.629175078952241,
9.42255501604705));
#10724=CARTESIAN_POINT('Ctrl Pts',(-1.00883395642591,0.110553388403418,
9.44531583505166));
#10725=CARTESIAN_POINT('Ctrl Pts',(-0.914753666531486,-0.443981321671508,
9.4681199191005));
#10726=CARTESIAN_POINT('Ctrl Pts',(-0.53935346555354,-0.864287702720483,
9.49096779294908));
#10727=CARTESIAN_POINT('Ctrl Pts',(0.00317473919602999,-1.02074393938534,
9.51385987936846));
#10728=CARTESIAN_POINT('Ctrl Pts',(0.546842451951703,-0.864277453369769,
9.53679662034949));
#10729=CARTESIAN_POINT('Ctrl Pts',(0.924675422089117,-0.441717222447211,
9.55977841069135));
#10730=CARTESIAN_POINT('Ctrl Pts',(1.01996808440899,0.118196481355525,9.58280563347303));
#10731=CARTESIAN_POINT('Ctrl Pts',(0.802331121841736,0.64402993935177,9.6058786398591));
#10732=CARTESIAN_POINT('Ctrl Pts',(0.337364397173406,0.974133999160165,
9.62899775887225));
#10733=CARTESIAN_POINT('Ctrl Pts',(-0.233104637031958,1.00632652768241,
9.65216329850443));
#10734=CARTESIAN_POINT('Ctrl Pts',(-0.734273786426299,0.729521681583079,
9.67537552627366));
#10735=CARTESIAN_POINT('Ctrl Pts',(-1.01192271602118,0.227485149733832,
9.69863471831026));
#10736=CARTESIAN_POINT('Ctrl Pts',(-0.979861010625463,-0.346471505307732,
9.72194105790298));
#10737=CARTESIAN_POINT('Ctrl Pts',(-0.646687232733913,-0.816385458535924,
9.74529485019366));
#10738=CARTESIAN_POINT('Ctrl Pts',(-0.113515831859443,-1.03740747700115,
9.76869605816828));
#10739=CARTESIAN_POINT('Ctrl Pts',(0.45666043399166,-0.940854540198569,
9.79214533421283));
#10740=CARTESIAN_POINT('Ctrl Pts',(0.888877742368337,-0.554658268165104,
9.8156417140768));
#10741=CARTESIAN_POINT('Ctrl Pts',(0.996072925475586,-0.183171021132321,
9.83133914183944));
#10742=CARTESIAN_POINT('Ctrl Pts',(0.996098069974061,0.00360871894456211,
9.83919327538718));
#10743=CARTESIAN_POINT('Ctrl Pts',(1.03719675406882,-0.00324058202589225,
7.35218360836862));
#10744=CARTESIAN_POINT('Ctrl Pts',(1.03717058144385,0.191176320370734,7.36035888637736));
#10745=CARTESIAN_POINT('Ctrl Pts',(0.925557853409022,0.578088834603603,
7.37670781473685));
#10746=CARTESIAN_POINT('Ctrl Pts',(0.47537110567802,0.980347295995417,7.40118088192312));
#10747=CARTESIAN_POINT('Ctrl Pts',(-0.118659904383316,1.08096987560822,
7.42561186891184));
#10748=CARTESIAN_POINT('Ctrl Pts',(-0.674264766014723,0.850659477558785,
7.4499972894827));
#10749=CARTESIAN_POINT('Ctrl Pts',(-1.0215282433438,0.360895066694614,7.47433816416247));
#10750=CARTESIAN_POINT('Ctrl Pts',(-1.05495989572618,-0.237418239847793,
7.49863351661875));
#10751=CARTESIAN_POINT('Ctrl Pts',(-0.765493965690148,-0.760837611247353,
7.52288328690495));
#10752=CARTESIAN_POINT('Ctrl Pts',(-0.242921801622797,-1.0494710437018,
7.54708703215697));
#10753=CARTESIAN_POINT('Ctrl Pts',(0.351970225278986,-1.01590502989561,
7.57124451032626));
#10754=CARTESIAN_POINT('Ctrl Pts',(0.836883375362913,-0.67164669764715,
7.59535542482914));
#10755=CARTESIAN_POINT('Ctrl Pts',(1.06386470149691,-0.123233424848443,
7.61941953772808));
#10756=CARTESIAN_POINT('Ctrl Pts',(0.96448818932038,0.460735663933303,7.64343662004129));
#10757=CARTESIAN_POINT('Ctrl Pts',(0.570400865876502,0.901456165300417,
7.66740647649098));
#10758=CARTESIAN_POINT('Ctrl Pts',(0.00343128420266171,1.06462402223465,
7.69132893385857));
#10759=CARTESIAN_POINT('Ctrl Pts',(-0.562462013634023,0.901470864308901,
7.71520384653006));
#10760=CARTESIAN_POINT('Ctrl Pts',(-0.93920407838125,0.479325471899194,
7.73814860418777));
#10761=CARTESIAN_POINT('Ctrl Pts',(-1.04563381734369,-0.0487591387118346,
7.76016910772723));
#10762=CARTESIAN_POINT('Ctrl Pts',(-0.893388715718348,-0.541954927211641,
7.78127102299369));
#10763=CARTESIAN_POINT('Ctrl Pts',(-0.524509993111373,-0.901534190695079,
7.80233509266462));
#10764=CARTESIAN_POINT('Ctrl Pts',(-0.0292887386476584,-1.04113014278304,
7.82336134357856));
#10765=CARTESIAN_POINT('Ctrl Pts',(0.470719775145307,-0.926199174985292,
7.84434971997527));
#10766=CARTESIAN_POINT('Ctrl Pts',(0.920151044870203,-0.531393688850765,
7.86879213004602));
#10767=CARTESIAN_POINT('Ctrl Pts',(1.07869587043031,0.159420004343398,7.89666351654933));
#10768=CARTESIAN_POINT('Ctrl Pts',(0.723895499075924,0.770663707163572,
7.92445965347429));
#10769=CARTESIAN_POINT('Ctrl Pts',(0.182030232236923,1.01363048371111,7.948726105815));
#10770=CARTESIAN_POINT('Ctrl Pts',(-0.324136171745627,0.975741615999532,
7.96948836497335));
#10771=CARTESIAN_POINT('Ctrl Pts',(-0.714453631350278,0.723213312087363,
7.98848651554928));
#10772=CARTESIAN_POINT('Ctrl Pts',(-0.935497699150504,0.370852328564716,
8.00573022282306));
#10773=CARTESIAN_POINT('Ctrl Pts',(-1.00520551147936,0.003280843936954,
8.02122871265022));
#10774=CARTESIAN_POINT('Ctrl Pts',(-0.935399570902944,-0.363301629637604,
8.03670639912639));
#10775=CARTESIAN_POINT('Ctrl Pts',(-0.671741170896316,-0.785473331547596,
8.05731555952276));
#10776=CARTESIAN_POINT('Ctrl Pts',(-0.0835914591230814,-1.06937590558802,
8.08302618007272));
#10777=CARTESIAN_POINT('Ctrl Pts',(0.664820094277504,-0.838174757202306,
8.11379655253259));
#10778=CARTESIAN_POINT('Ctrl Pts',(1.05441848069546,-0.161982020970417,
8.14448592141602));
#10779=CARTESIAN_POINT('Ctrl Pts',(0.881123855699413,0.596820461156313,
8.17509503429765));
#10780=CARTESIAN_POINT('Ctrl Pts',(0.238762774028777,1.03430920701819,8.20562474600236));
#10781=CARTESIAN_POINT('Ctrl Pts',(-0.440989874038897,0.930485897466661,
8.23269309303528));
#10782=CARTESIAN_POINT('Ctrl Pts',(-0.854200921270452,0.525410375048001,
8.25632711980103));
#10783=CARTESIAN_POINT('Ctrl Pts',(-1.00008100917318,0.0531416845693213,
8.27655112488305));
#10784=CARTESIAN_POINT('Ctrl Pts',(-0.90200349917642,-0.431042585830742,
8.29674152510973));
#10785=CARTESIAN_POINT('Ctrl Pts',(-0.585232908856582,-0.808836535644948,
8.31689817148631));
#10786=CARTESIAN_POINT('Ctrl Pts',(-0.241484208369084,-0.943331975688694,
8.33199166132556));
#10787=CARTESIAN_POINT('Ctrl Pts',(-0.00313258390604597,-0.958028426645384,
8.34204308984535));
#10788=CARTESIAN_POINT('Ctrl Pts',(0.155630995470786,-0.948146354918541,
8.34874143218627));
#10789=CARTESIAN_POINT('Ctrl Pts',(0.388406644952516,-0.889043212840594,
8.35878305450209));
#10790=CARTESIAN_POINT('Ctrl Pts',(0.660946080093702,-0.717199923829581,
8.37215894305961));
#10791=CARTESIAN_POINT('Ctrl Pts',(0.949982129920854,-0.328582950010552,
8.39219849402223));
#10792=CARTESIAN_POINT('Ctrl Pts',(0.998559015277984,0.304265589788258,
8.41720373230134));
#10793=CARTESIAN_POINT('Ctrl Pts',(0.522077893834886,0.900628246456589,
8.44714268357634));
#10794=CARTESIAN_POINT('Ctrl Pts',(-0.165513598662709,1.00284693060682,
8.4745244155206));
#10795=CARTESIAN_POINT('Ctrl Pts',(-0.701855624130506,0.705135890791863,
8.49936815983874));
#10796=CARTESIAN_POINT('Ctrl Pts',(-0.967948575818185,0.223795924594876,
8.52169152062583));
#10797=CARTESIAN_POINT('Ctrl Pts',(-0.93711414110698,-0.325536385888489,
8.54397906340804));
#10798=CARTESIAN_POINT('Ctrl Pts',(-0.67803860118516,-0.6895070937393,8.56211163922283));
#10799=CARTESIAN_POINT('Ctrl Pts',(-0.325363913511247,-0.905040920367593,
8.57939955057773));
#10800=CARTESIAN_POINT('Ctrl Pts',(0.0309053846454797,-0.967971730440252,
8.59420275005887));
#10801=CARTESIAN_POINT('Ctrl Pts',(0.413941925614915,-0.864842868973118,
8.61063250335662));
#10802=CARTESIAN_POINT('Ctrl Pts',(0.700715405917063,-0.653424071291302,
8.62540408573038));
#10803=CARTESIAN_POINT('Ctrl Pts',(0.890003605091469,-0.351808044165019,
8.64016247285312));
#10804=CARTESIAN_POINT('Ctrl Pts',(0.967542406534895,0.0559962531859067,
8.65736364651605));
#10805=CARTESIAN_POINT('Ctrl Pts',(0.833760313033866,0.521285133638719,
8.67700070139823));
#10806=CARTESIAN_POINT('Ctrl Pts',(0.42782549810846,0.883792680066817,8.69906186563957));
#10807=CARTESIAN_POINT('Ctrl Pts',(-0.107804311833239,0.974704985814576,
8.72109429595876));
#10808=CARTESIAN_POINT('Ctrl Pts',(-0.609174652584766,0.766947011662965,
8.7430985571953));
#10809=CARTESIAN_POINT('Ctrl Pts',(-0.922729261913642,0.324844912449117,
8.76507576134807));
#10810=CARTESIAN_POINT('Ctrl Pts',(-0.952999507734519,-0.215677498529127,
8.78702678544552));
#10811=CARTESIAN_POINT('Ctrl Pts',(-0.691348090308507,-0.688911833502101,
8.80895262586299));
#10812=CARTESIAN_POINT('Ctrl Pts',(-0.218553588797013,-0.950119550572946,
8.83085424324479));
#10813=CARTESIAN_POINT('Ctrl Pts',(0.32017377908378,-0.919784087573411,
8.85273263486959));
#10814=CARTESIAN_POINT('Ctrl Pts',(0.759744995635515,-0.607799082156627,
8.87458879663461));
#10815=CARTESIAN_POINT('Ctrl Pts',(0.965755577871433,-0.11025296341866,
8.89642374112683));
#10816=CARTESIAN_POINT('Ctrl Pts',(0.875579662109175,0.420143968732924,
8.91823850470675));
#10817=CARTESIAN_POINT('Ctrl Pts',(0.517338405956845,0.820918470026088,
8.94003411305096));
#10818=CARTESIAN_POINT('Ctrl Pts',(0.0012710543841073,0.969544978443646,
8.96181165944999));
#10819=CARTESIAN_POINT('Ctrl Pts',(-0.514464942965089,0.820953664757525,
8.98357213567796));
#10820=CARTESIAN_POINT('Ctrl Pts',(-0.858337283734613,0.435843869483925,
9.00451148214707));
#10821=CARTESIAN_POINT('Ctrl Pts',(-0.955560714905759,-0.0466269226500807,
9.02463212714799));
#10822=CARTESIAN_POINT('Ctrl Pts',(-0.816688402207661,-0.497728249872681,
9.04393592539421));
#10823=CARTESIAN_POINT('Ctrl Pts',(-0.506889147550573,-0.799878736533962,
9.06162207865932));
#10824=CARTESIAN_POINT('Ctrl Pts',(-0.14096336145598,-0.927213398264503,
9.07769385094099));
#10825=CARTESIAN_POINT('Ctrl Pts',(0.324512190886538,-0.911102185093492,
9.09697223469682));
#10826=CARTESIAN_POINT('Ctrl Pts',(0.728968813708346,-0.636669415745461,
9.11624302783002));
#10827=CARTESIAN_POINT('Ctrl Pts',(0.91324192523573,-0.2091896101292,9.13550450393053));
#10828=CARTESIAN_POINT('Ctrl Pts',(0.932302842350122,0.254831083543151,
9.15476058856452));
#10829=CARTESIAN_POINT('Ctrl Pts',(0.626900263580331,0.785504982864274,
9.17882483506651));
#10830=CARTESIAN_POINT('Ctrl Pts',(0.0423452694845425,0.964740415964174,
9.20287985836102));
#10831=CARTESIAN_POINT('Ctrl Pts',(-0.405906098755213,0.843205768511259,
9.22211803373898));
#10832=CARTESIAN_POINT('Ctrl Pts',(-0.717235768498481,0.614120703650391,
9.23814771688336));
#10833=CARTESIAN_POINT('Ctrl Pts',(-0.92370760684931,0.235266265275963,
9.25578020037257));
#10834=CARTESIAN_POINT('Ctrl Pts',(-0.923376422631151,-0.235005878724949,
9.27501174354034));
#10835=CARTESIAN_POINT('Ctrl Pts',(-0.698715298937986,-0.648292214447006,
9.29424327143548));
#10836=CARTESIAN_POINT('Ctrl Pts',(-0.303406202904001,-0.903192481821634,
9.31347490228703));
#10837=CARTESIAN_POINT('Ctrl Pts',(0.16559811215366,-0.938655265798546,
9.33270600943893));
#10838=CARTESIAN_POINT('Ctrl Pts',(0.491608636905682,-0.791338058660878,
9.34733350869031));
#10839=CARTESIAN_POINT('Ctrl Pts',(0.666820161878111,-0.630086196708776,
9.35735100901671));
#10840=CARTESIAN_POINT('Ctrl Pts',(0.775546109169976,-0.497595093735688,
9.3645640119917));
#10841=CARTESIAN_POINT('Ctrl Pts',(0.914746049094079,-0.229100519953174,
9.37718769779949));
#10842=CARTESIAN_POINT('Ctrl Pts',(0.934696371728414,0.12593490391397,9.3916192338851));
#10843=CARTESIAN_POINT('Ctrl Pts',(0.810930047844375,0.448675148178548,
9.4060507946647));
#10844=CARTESIAN_POINT('Ctrl Pts',(0.603540213098328,0.725122428597784,
9.42048450263819));
#10845=CARTESIAN_POINT('Ctrl Pts',(0.214205829944543,0.940615684273133,
9.43853221348709));
#10846=CARTESIAN_POINT('Ctrl Pts',(-0.31933594831027,0.910615224040587,
9.460195939325));
#10847=CARTESIAN_POINT('Ctrl Pts',(-0.755217739844288,0.601392195346104,
9.48186844163729));
#10848=CARTESIAN_POINT('Ctrl Pts',(-0.959902232150957,0.10736858445662,
9.50355036655641));
#10849=CARTESIAN_POINT('Ctrl Pts',(-0.870316378158485,-0.420063150575497,
9.52524306057417));
#10850=CARTESIAN_POINT('Ctrl Pts',(-0.51366548932194,-0.819226222680466,
9.54694754310527));
#10851=CARTESIAN_POINT('Ctrl Pts',(0.00099722262819886,-0.967543954202361,
9.56866494808632));
#10852=CARTESIAN_POINT('Ctrl Pts',(0.516016920582239,-0.81922256521234,
9.5903963601957));
#10853=CARTESIAN_POINT('Ctrl Pts',(0.873436814265292,-0.419352238605789,
9.61214286014485));
#10854=CARTESIAN_POINT('Ctrl Pts',(0.963398958340639,0.10977813142819,9.63390552377525));
#10855=CARTESIAN_POINT('Ctrl Pts',(0.757897894439999,0.606061766756622,
9.65568540741735));
#10856=CARTESIAN_POINT('Ctrl Pts',(0.319489023351443,0.9172073481515,9.67748356901533));
#10857=CARTESIAN_POINT('Ctrl Pts',(-0.217739692090491,0.947441559483756,
9.69930104654587));
#10858=CARTESIAN_POINT('Ctrl Pts',(-0.689154860322401,0.686979141731466,
9.72113887780304));
#10859=CARTESIAN_POINT('Ctrl Pts',(-0.950001674292135,0.215160715023784,
9.74299805428903));
#10860=CARTESIAN_POINT('Ctrl Pts',(-0.919826616460147,-0.323661293630411,
9.76487966279437));
#10861=CARTESIAN_POINT('Ctrl Pts',(-0.607283029397313,-0.764355668580401,
9.78678450836089));
#10862=CARTESIAN_POINT('Ctrl Pts',(-0.107654549029002,-0.971392889114284,
9.80871400622512));
#10863=CARTESIAN_POINT('Ctrl Pts',(0.426152293844201,-0.880962937933544,
9.8306681505383));
#10864=CARTESIAN_POINT('Ctrl Pts',(0.830424803659154,-0.519624647538494,
9.85265006399591));
#10865=CARTESIAN_POINT('Ctrl Pts',(0.930600595159381,-0.172510125317866,
9.86731890233875));
#10866=CARTESIAN_POINT('Ctrl Pts',(0.930624104877249,0.00212604796771284,
9.87466239594617));
#10867=CARTESIAN_POINT('Ctrl Pts',(1.08384642846031,-0.000793256800902784,
7.29413292869025));
#10868=CARTESIAN_POINT('Ctrl Pts',(1.08381908929503,0.202289003082833,7.30267258708788));
#10869=CARTESIAN_POINT('Ctrl Pts',(0.967159117688111,0.606890912023917,
7.31977033977986));
#10870=CARTESIAN_POINT('Ctrl Pts',(0.495930087867846,1.02807430064273,7.34539171275669));
#10871=CARTESIAN_POINT('Ctrl Pts',(-0.126761042383259,1.13367938470921,
7.37100435156813));
#10872=CARTESIAN_POINT('Ctrl Pts',(-0.709971284708507,0.892049379954826,
7.39660097985035));
#10873=CARTESIAN_POINT('Ctrl Pts',(-1.07501405252591,0.377418129162179,
7.42218333959883));
#10874=CARTESIAN_POINT('Ctrl Pts',(-1.11030586598071,-0.252127576999562,
7.4477491320311));
#10875=CARTESIAN_POINT('Ctrl Pts',(-0.805456401016912,-0.803593486480699,
7.47329786737596));
#10876=CARTESIAN_POINT('Ctrl Pts',(-0.254335423454531,-1.10811832577815,
7.4988282519598));
#10877=CARTESIAN_POINT('Ctrl Pts',(0.373850028247498,-1.07277814526268,
7.52433935505151));
#10878=CARTESIAN_POINT('Ctrl Pts',(0.886537206986384,-0.708926672984277,
7.54983010396061));
#10879=CARTESIAN_POINT('Ctrl Pts',(1.12684930546936,-0.128563840777488,
7.57529949924907));
#10880=CARTESIAN_POINT('Ctrl Pts',(1.02165804861735,0.490150925268269,7.6007465283239));
#10881=CARTESIAN_POINT('Ctrl Pts',(0.603764038088763,0.957636470965819,
7.62617019061896));
#10882=CARTESIAN_POINT('Ctrl Pts',(0.00185210167093897,1.13095496972185,
7.65156953889001));
#10883=CARTESIAN_POINT('Ctrl Pts',(-0.59956549271009,0.9576526886088,7.67694353645162));
#10884=CARTESIAN_POINT('Ctrl Pts',(-1.00039059858681,0.508644588622468,
7.70135260850433));
#10885=CARTESIAN_POINT('Ctrl Pts',(-1.11376643951718,-0.0535942367798588,
7.72479874105888));
#10886=CARTESIAN_POINT('Ctrl Pts',(-0.951594070937359,-0.579139877751677,
7.74728507022348));
#10887=CARTESIAN_POINT('Ctrl Pts',(-0.558264880040219,-0.962633038967035,
7.76974846765362));
#10888=CARTESIAN_POINT('Ctrl Pts',(-0.0297845563498375,-1.11165847490554,
7.79218801827507));
#10889=CARTESIAN_POINT('Ctrl Pts',(0.504224144516551,-0.988964719556773,
7.8146035994472));
#10890=CARTESIAN_POINT('Ctrl Pts',(0.984577474321374,-0.56707344670203,
7.84072646125844));
#10891=CARTESIAN_POINT('Ctrl Pts',(1.15430617570018,0.171814819585418,7.87054013838732));
#10892=CARTESIAN_POINT('Ctrl Pts',(0.774547719067364,0.826325866763944,
7.90030160483131));
#10893=CARTESIAN_POINT('Ctrl Pts',(0.193979612614955,1.08670118860458,7.9263023705649));
#10894=CARTESIAN_POINT('Ctrl Pts',(-0.348665393370604,1.04611990516275,
7.94856102173379));
#10895=CARTESIAN_POINT('Ctrl Pts',(-0.767359045720052,0.775275157221321,
7.9689396492515));
#10896=CARTESIAN_POINT('Ctrl Pts',(-1.00458183390253,0.397155764877826,
7.98744444059531));
#10897=CARTESIAN_POINT('Ctrl Pts',(-1.07942987205928,0.00256356478130836,
8.00408248537729));
#10898=CARTESIAN_POINT('Ctrl Pts',(-1.0044783210053,-0.391111487886477,
8.02070397667786));
#10899=CARTESIAN_POINT('Ctrl Pts',(-0.721260789217433,-0.844639481874048,
8.04284350578955));
#10900=CARTESIAN_POINT('Ctrl Pts',(-0.0891736393931901,-1.14984162670411,
8.0704763974833));
#10901=CARTESIAN_POINT('Ctrl Pts',(0.715678720844839,-0.901299501303157,
8.1035658986358));
#10902=CARTESIAN_POINT('Ctrl Pts',(1.13492007912664,-0.17381149421113,8.13658458374464));
#10903=CARTESIAN_POINT('Ctrl Pts',(0.948455032144445,0.64295968933924,8.16953075755057));
#10904=CARTESIAN_POINT('Ctrl Pts',(0.256816826853416,1.11407722004625,8.20240312942989));
#10905=CARTESIAN_POINT('Ctrl Pts',(-0.475327032992583,1.00229310544698,
8.23155630552289));
#10906=CARTESIAN_POINT('Ctrl Pts',(-0.920474247117944,0.565929865334376,
8.25701571321748));
#10907=CARTESIAN_POINT('Ctrl Pts',(-1.07765167819056,0.0571232220460662,
8.27880380868564));
#10908=CARTESIAN_POINT('Ctrl Pts',(-0.971985175738061,-0.464564051003078,
8.30055729936963));
#10909=CARTESIAN_POINT('Ctrl Pts',(-0.630665261642236,-0.871644705172118,
8.32227584244456));
#10910=CARTESIAN_POINT('Ctrl Pts',(-0.260275322606424,-1.01656300716899,
8.33853832228072));
#10911=CARTESIAN_POINT('Ctrl Pts',(-0.00344558452418022,-1.0323993719803,
8.34936892151002));
#10912=CARTESIAN_POINT('Ctrl Pts',(0.167623965316464,-1.02175149523021,
8.35658635286812));
#10913=CARTESIAN_POINT('Ctrl Pts',(0.418436678562632,-0.958069044630896,
8.36740579432199));
#10914=CARTESIAN_POINT('Ctrl Pts',(0.712079660427613,-0.7729198568326,8.3818167331061));
#10915=CARTESIAN_POINT('Ctrl Pts',(1.02347973785374,-0.354227798098456,
8.40340626006335));
#10916=CARTESIAN_POINT('Ctrl Pts',(1.07578845759894,0.327516652661325,8.43034229555736));
#10917=CARTESIAN_POINT('Ctrl Pts',(0.562588863844005,0.969761430420295,
8.46258290726966));
#10918=CARTESIAN_POINT('Ctrl Pts',(-0.177715492101827,1.07977400632615,
8.49206088659617));
#10919=CARTESIAN_POINT('Ctrl Pts',(-0.754969512302287,0.759321620849947,
8.51879847856748));
#10920=CARTESIAN_POINT('Ctrl Pts',(-1.04125073281678,0.241419209252838,
8.54281498297182));
#10921=CARTESIAN_POINT('Ctrl Pts',(-1.00805722180633,-0.349404771948186,
8.56678423739501));
#10922=CARTESIAN_POINT('Ctrl Pts',(-0.729517853526143,-0.740677351451125,
8.58627564980444));
#10923=CARTESIAN_POINT('Ctrl Pts',(-0.350480132340932,-0.972316810663511,
8.60485496723001));
#10924=CARTESIAN_POINT('Ctrl Pts',(0.0322991958263789,-1.03990993998121,
8.62075891439363));
#10925=CARTESIAN_POINT('Ctrl Pts',(0.443650471011225,-0.929143712575293,
8.63840200647036));
#10926=CARTESIAN_POINT('Ctrl Pts',(0.751518738327972,-0.702159843963306,
8.6542599534087));
#10927=CARTESIAN_POINT('Ctrl Pts',(0.954636456966557,-0.37848104417437,
8.67009604620781));
#10928=CARTESIAN_POINT('Ctrl Pts',(1.03779888771484,0.0589833027264458,
8.68854704443214));
#10929=CARTESIAN_POINT('Ctrl Pts',(0.894321819630977,0.557814720788599,
8.7095975416509));
#10930=CARTESIAN_POINT('Ctrl Pts',(0.459360346577918,0.946166909345621,
8.73323177261074));
#10931=CARTESIAN_POINT('Ctrl Pts',(-0.114118824404391,1.04344007211952,
8.75681788745377));
#10932=CARTESIAN_POINT('Ctrl Pts',(-0.650476848794739,0.82111535279448,
8.78035613912247));
#10933=CARTESIAN_POINT('Ctrl Pts',(-0.985604987995532,0.348480992052307,
8.80384648245865));
#10934=CARTESIAN_POINT('Ctrl Pts',(-1.01786740958942,-0.228839867930964,
8.82728905034341));
#10935=CARTESIAN_POINT('Ctrl Pts',(-0.738589557901741,-0.733806334779716,
8.85068393868067));
#10936=CARTESIAN_POINT('Ctrl Pts',(-0.234488932120026,-1.01222446231625,
8.87403130042571));
#10937=CARTESIAN_POINT('Ctrl Pts',(0.339309874015096,-0.979835882831324,
8.89733130405925));
#10938=CARTESIAN_POINT('Ctrl Pts',(0.806983157414378,-0.647805656061189,
8.920584146721));
#10939=CARTESIAN_POINT('Ctrl Pts',(1.02587940738221,-0.11891857779353,8.94379005403647));
#10940=CARTESIAN_POINT('Ctrl Pts',(0.930047505375005,0.444228970333776,
8.9669492663554));
#10941=CARTESIAN_POINT('Ctrl Pts',(0.550037348365757,0.869224147485282,
8.99006207126683));
#10942=CARTESIAN_POINT('Ctrl Pts',(0.00331688177892927,1.02658582996463,
9.01312872078293));
#10943=CARTESIAN_POINT('Ctrl Pts',(-0.542345277424951,0.869275726604705,
9.03614961115852));
#10944=CARTESIAN_POINT('Ctrl Pts',(-0.905667395299237,0.4622482747292,9.05827393317691));
#10945=CARTESIAN_POINT('Ctrl Pts',(-1.00821264225331,-0.047010260451699,
9.07950822199612));
#10946=CARTESIAN_POINT('Ctrl Pts',(-0.861732962585674,-0.522594137999902,
9.09985879309251));
#10947=CARTESIAN_POINT('Ctrl Pts',(-0.535452731740728,-0.840721246165385,
9.11848100566275));
#10948=CARTESIAN_POINT('Ctrl Pts',(-0.150527266233238,-0.974636173165108,
9.13538461085382));
#10949=CARTESIAN_POINT('Ctrl Pts',(0.338682804184835,-0.957648390576258,
9.15564420037776));
#10950=CARTESIAN_POINT('Ctrl Pts',(0.76304477781549,-0.669506770040774,
9.1758634753981));
#10951=CARTESIAN_POINT('Ctrl Pts',(0.956095920089128,-0.221513534188684,
9.19604620427903));
#10952=CARTESIAN_POINT('Ctrl Pts',(0.976011877017348,0.26431211473213,9.2162043883441));
#10953=CARTESIAN_POINT('Ctrl Pts',(0.656548774825726,0.81891683061587,9.24135284185631));
#10954=CARTESIAN_POINT('Ctrl Pts',(0.0466882531800841,1.00566644796459,
9.26644056558201));
#10955=CARTESIAN_POINT('Ctrl Pts',(-0.420196777981749,0.879028902672049,
9.28647688240236));
#10956=CARTESIAN_POINT('Ctrl Pts',(-0.744120699223029,0.640630339035476,
9.30315438470658));
#10957=CARTESIAN_POINT('Ctrl Pts',(-0.95861694874501,0.246913067796348,
9.32147257780598));
#10958=CARTESIAN_POINT('Ctrl Pts',(-0.958178271491326,-0.241092352278578,
9.3414279620528));
#10959=CARTESIAN_POINT('Ctrl Pts',(-0.725325955917838,-0.669287711537651,
9.361352107215));
#10960=CARTESIAN_POINT('Ctrl Pts',(-0.31628593978967,-0.932926599228729,
9.3812463447098));
#10961=CARTESIAN_POINT('Ctrl Pts',(0.168249973887814,-0.969479581836067,
9.40111282491626));
#10962=CARTESIAN_POINT('Ctrl Pts',(0.504451373670123,-0.817462569521572,
9.4161945546897));
#10963=CARTESIAN_POINT('Ctrl Pts',(0.685009996862284,-0.6512836464409,9.42651766084202));
#10964=CARTESIAN_POINT('Ctrl Pts',(0.797005370990673,-0.514805420344457,
9.43394717676915));
#10965=CARTESIAN_POINT('Ctrl Pts',(0.940278681951758,-0.23840503025821,
9.44694090738106));
#10966=CARTESIAN_POINT('Ctrl Pts',(0.960696404399766,0.126535341586046,
9.46177038655293));
#10967=CARTESIAN_POINT('Ctrl Pts',(0.833607413309956,0.457875833720658,
9.47658602820858));
#10968=CARTESIAN_POINT('Ctrl Pts',(0.620852271531433,0.741434358704751,
9.49139014459053));
#10969=CARTESIAN_POINT('Ctrl Pts',(0.221996454884777,0.962065864953804,
9.50987237532345));
#10970=CARTESIAN_POINT('Ctrl Pts',(-0.323541174854107,0.931248882602088,
9.53201979030854));
#10971=CARTESIAN_POINT('Ctrl Pts',(-0.768333094902132,0.615525665216968,
9.55413527108079));
#10972=CARTESIAN_POINT('Ctrl Pts',(-0.976727100725712,0.112174129761956,
9.5762202682564));
#10973=CARTESIAN_POINT('Ctrl Pts',(-0.885486082363011,-0.424142120536936,
9.59827535662572));
#10974=CARTESIAN_POINT('Ctrl Pts',(-0.523378588106049,-0.829197320524031,
9.62030154695759));
#10975=CARTESIAN_POINT('Ctrl Pts',(-0.0019324619193897,-0.979320702375544,
9.64229967474914));
#10976=CARTESIAN_POINT('Ctrl Pts',(0.518815530859397,-0.829199944725929,
9.66427069811794));
#10977=CARTESIAN_POINT('Ctrl Pts',(0.87944912287424,-0.425517469831924,
9.68621553547096));
#10978=CARTESIAN_POINT('Ctrl Pts',(0.969932314485265,0.107543910523038,
9.70813515474387));
#10979=CARTESIAN_POINT('Ctrl Pts',(0.763171810925342,0.606487765894584,
9.73003051320366));
#10980=CARTESIAN_POINT('Ctrl Pts',(0.323116327168651,0.918622711733031,
9.75190260774064));
#10981=CARTESIAN_POINT('Ctrl Pts',(-0.215009582857648,0.948761113833324,
9.77375241361181));
#10982=CARTESIAN_POINT('Ctrl Pts',(-0.686236351315572,0.688237658598508,
9.79558097984185));
#10983=CARTESIAN_POINT('Ctrl Pts',(-0.946396968696602,0.217366324799682,
9.81738921471157));
#10984=CARTESIAN_POINT('Ctrl Pts',(-0.916205377388286,-0.319261288483713,
9.83917839754132));
#10985=CARTESIAN_POINT('Ctrl Pts',(-0.605414027709865,-0.757254947166093,
9.86094896999974));
#10986=CARTESIAN_POINT('Ctrl Pts',(-0.109657320635582,-0.962534333662517,
9.88270327490055));
#10987=CARTESIAN_POINT('Ctrl Pts',(0.418914924439416,-0.872861288741235,
9.90443938873523));
#10988=CARTESIAN_POINT('Ctrl Pts',(0.818388829673488,-0.51557521947165,
9.92616491491646));
#10989=CARTESIAN_POINT('Ctrl Pts',(0.917073865342883,-0.173169092744639,
9.94062996432396));
#10990=CARTESIAN_POINT('Ctrl Pts',(0.917097049589342,-0.000950604005939382,
9.94787179370752));
#10991=CARTESIAN_POINT('Ctrl Pts',(1.0670179066401,0.00225746580351556,
7.22152958911222));
#10992=CARTESIAN_POINT('Ctrl Pts',(1.06699097611627,0.202304233294702,7.2299416043168));
#10993=CARTESIAN_POINT('Ctrl Pts',(0.952169493387724,0.600953273779197,
7.24678378615139));
#10994=CARTESIAN_POINT('Ctrl Pts',(0.487186394855587,1.01678373272383,7.27207042045906));
#10995=CARTESIAN_POINT('Ctrl Pts',(-0.128346163220755,1.12129993252972,
7.29738651367873));
#10996=CARTESIAN_POINT('Ctrl Pts',(-0.705870567011168,0.882175433229343,
7.32272911076493));
#10997=CARTESIAN_POINT('Ctrl Pts',(-1.0680195677792,0.371849003294253,7.34809819670836));
#10998=CARTESIAN_POINT('Ctrl Pts',(-1.10321422557632,-0.253530752930648,
7.37349240932164));
#10999=CARTESIAN_POINT('Ctrl Pts',(-0.800005714726182,-0.802315846496021,
7.39891096663443));
#11000=CARTESIAN_POINT('Ctrl Pts',(-0.250806475805171,-1.10594008465963,
7.42435280627046));
#11001=CARTESIAN_POINT('Ctrl Pts',(0.376295106921614,-1.07080374820359,
7.4498169663272));
#11002=CARTESIAN_POINT('Ctrl Pts',(0.889008624586151,-0.707108832454598,
7.47530242608526));
#11003=CARTESIAN_POINT('Ctrl Pts',(1.12981834509025,-0.125917689478273,
7.50080817431521));
#11004=CARTESIAN_POINT('Ctrl Pts',(1.02443603606273,0.494773142194464,7.52633316714341));
#11005=CARTESIAN_POINT('Ctrl Pts',(0.604646428898813,0.964593536017731,
7.55187637605968));
#11006=CARTESIAN_POINT('Ctrl Pts',(-0.00109375463389684,1.13916272997907,
7.57743671976539));
#11007=CARTESIAN_POINT('Ctrl Pts',(-0.607399194221062,0.964601513127144,
7.60301318476041));
#11008=CARTESIAN_POINT('Ctrl Pts',(-1.01221199749175,0.511330398063977,
7.62765674322727));
#11009=CARTESIAN_POINT('Ctrl Pts',(-1.12696398058896,-0.0572091674480348,
7.65136486655048));
#11010=CARTESIAN_POINT('Ctrl Pts',(-0.962827544625284,-0.589451999852308,
7.67413480745332));
#11011=CARTESIAN_POINT('Ctrl Pts',(-0.56400406423614,-0.978430974917163,
7.69691430442555));
#11012=CARTESIAN_POINT('Ctrl Pts',(-0.0273139330862592,-1.12987903202044,
7.71970276832014));
#11013=CARTESIAN_POINT('Ctrl Pts',(0.515815112770866,-1.00518016474251,
7.74249910058463));
#11014=CARTESIAN_POINT('Ctrl Pts',(1.00510855649337,-0.575600695245217,
7.76910313379358));
#11015=CARTESIAN_POINT('Ctrl Pts',(1.17855810364818,0.178171254926354,7.79951779751799));
#11016=CARTESIAN_POINT('Ctrl Pts',(0.790555243745666,0.847481198951724,
7.82994286951095));
#11017=CARTESIAN_POINT('Ctrl Pts',(0.195989759376802,1.11426017821105,7.85657119093045));
#11018=CARTESIAN_POINT('Ctrl Pts',(-0.360542451510464,1.072730591672,7.87939875619507));
#11019=CARTESIAN_POINT('Ctrl Pts',(-0.790575610104427,0.794655665848824,
7.90032600950703));
#11020=CARTESIAN_POINT('Ctrl Pts',(-1.03452330807482,0.405894124045869,
7.91935211503271));
#11021=CARTESIAN_POINT('Ctrl Pts',(-1.11159730313937,-0.000226215064824152,
7.93647617919723));
#11022=CARTESIAN_POINT('Ctrl Pts',(-1.03440926459159,-0.405828742159562,
7.95360049379582));
#11023=CARTESIAN_POINT('Ctrl Pts',(-0.74237760663053,-0.87357549827158,
7.97643284086373));
#11024=CARTESIAN_POINT('Ctrl Pts',(-0.0896511524093107,-1.18902475277104,
8.00497202233576));
#11025=CARTESIAN_POINT('Ctrl Pts',(0.743363174455746,-0.932124406438126,
8.03921482596584));
#11026=CARTESIAN_POINT('Ctrl Pts',(1.17833662686497,-0.177955302960707,
8.0734505711755));
#11027=CARTESIAN_POINT('Ctrl Pts',(0.984923832475398,0.670619764075562,
8.10767668130492));
#11028=CARTESIAN_POINT('Ctrl Pts',(0.265230218108454,1.16122051794983,8.14189039895527));
#11029=CARTESIAN_POINT('Ctrl Pts',(-0.498244706977025,1.04490742079478,
8.17228939848879));
#11030=CARTESIAN_POINT('Ctrl Pts',(-0.96319243578791,0.589275579142102,
8.19887688574252));
#11031=CARTESIAN_POINT('Ctrl Pts',(-1.1276004842514,0.0573158710798558,
8.22165762197572));
#11032=CARTESIAN_POINT('Ctrl Pts',(-1.01706918705279,-0.488791893957402,
8.24442896924834));
#11033=CARTESIAN_POINT('Ctrl Pts',(-0.65942985328418,-0.9154574609399,8.26718997588247));
#11034=CARTESIAN_POINT('Ctrl Pts',(-0.270837562173685,-1.06755876416323,
8.28425279203188));
#11035=CARTESIAN_POINT('Ctrl Pts',(-0.00118687354693406,-1.08418781783305,
8.29562403461343));
#11036=CARTESIAN_POINT('Ctrl Pts',(0.17847181968188,-1.07300615066178,8.30320390908866));
#11037=CARTESIAN_POINT('Ctrl Pts',(0.441991001954779,-1.00610838488519,
8.31457153222276));
#11038=CARTESIAN_POINT('Ctrl Pts',(0.750736604364479,-0.811461732201089,
8.3297233770891));
#11039=CARTESIAN_POINT('Ctrl Pts',(1.07843616258299,-0.370936248534933,
8.35244115703416));
#11040=CARTESIAN_POINT('Ctrl Pts',(1.13374581637679,0.347265474782159,8.38081929419995));
#11041=CARTESIAN_POINT('Ctrl Pts',(0.592433182066138,1.02511972772588,8.41484104544098));
#11042=CARTESIAN_POINT('Ctrl Pts',(-0.189892820508684,1.14158783659837,
8.44599497305806));
#11043=CARTESIAN_POINT('Ctrl Pts',(-0.800772820980421,0.802593366402982,
8.47428867201138));
#11044=CARTESIAN_POINT('Ctrl Pts',(-1.10410464127913,0.254019264636482,
8.49973091044463));
#11045=CARTESIAN_POINT('Ctrl Pts',(-1.06899657652552,-0.372507568119275,
8.52514967281803));
#11046=CARTESIAN_POINT('Ctrl Pts',(-0.7733700537891,-0.787895550254676,
8.54584195730769));
#11047=CARTESIAN_POINT('Ctrl Pts',(-0.370740708663388,-1.03396781530568,
8.56557858405426));
#11048=CARTESIAN_POINT('Ctrl Pts',(0.036128362188144,-1.10585716589204,
8.58248423797523));
#11049=CARTESIAN_POINT('Ctrl Pts',(0.473720894744957,-0.988052361384637,
8.60125353364536));
#11050=CARTESIAN_POINT('Ctrl Pts',(0.80142920960278,-0.746466523315921,
8.61813325756913));
#11051=CARTESIAN_POINT('Ctrl Pts',(1.01778681299134,-0.401731344034236,
8.63500132881749));
#11052=CARTESIAN_POINT('Ctrl Pts',(1.10643741011627,0.0644691098389064,
8.65466549145617));
#11053=CARTESIAN_POINT('Ctrl Pts',(0.953481848200125,0.596494435383873,
8.67711832298153));
#11054=CARTESIAN_POINT('Ctrl Pts',(0.489254428552112,1.01107283728095,8.7023473450177));
#11055=CARTESIAN_POINT('Ctrl Pts',(-0.123357404494991,1.11505446266801,
8.72754575370462));
#11056=CARTESIAN_POINT('Ctrl Pts',(-0.696794985125646,0.877430464208332,
8.75271243011979));
#11057=CARTESIAN_POINT('Ctrl Pts',(-1.05539207302399,0.371804106734305,
8.77784666980832));
#11058=CARTESIAN_POINT('Ctrl Pts',(-1.08999120326104,-0.246294887366169,
8.80294760364296));
#11059=CARTESIAN_POINT('Ctrl Pts',(-0.790831476581851,-0.7873228005966,
8.82801445891056));
#11060=CARTESIAN_POINT('Ctrl Pts',(-0.250437283560287,-1.08584491695925,
8.85304644391363));
#11061=CARTESIAN_POINT('Ctrl Pts',(0.365074934754753,-1.05115032210123,
8.87804279858019));
#11062=CARTESIAN_POINT('Ctrl Pts',(0.867054606378142,-0.694819513608586,
8.90300278281863));
#11063=CARTESIAN_POINT('Ctrl Pts',(1.1021587421701,-0.126881195388152,8.92792567275981));
#11064=CARTESIAN_POINT('Ctrl Pts',(0.999234894086778,0.478167753869344,
8.95281077626079));
#11065=CARTESIAN_POINT('Ctrl Pts',(0.59079348095087,0.935010182874376,8.97765740192141));
#11066=CARTESIAN_POINT('Ctrl Pts',(0.00289559293650473,1.10425340130915,
9.00246494193154));
#11067=CARTESIAN_POINT('Ctrl Pts',(-0.58410289937492,0.935052600972256,
9.02723269116248));
#11068=CARTESIAN_POINT('Ctrl Pts',(-0.975094294651602,0.497057410139674,
9.05104442397967));
#11069=CARTESIAN_POINT('Ctrl Pts',(-1.08549188235095,-0.0511126263223194,
9.0739041956868));
#11070=CARTESIAN_POINT('Ctrl Pts',(-0.927797132691072,-0.563142626479479,
9.09581584631526));
#11071=CARTESIAN_POINT('Ctrl Pts',(-0.576444633511331,-0.905731153030661,
9.11587150880217));
#11072=CARTESIAN_POINT('Ctrl Pts',(-0.16186322904714,-1.04996464479364,
9.13407984159281));
#11073=CARTESIAN_POINT('Ctrl Pts',(0.365077377739307,-1.03167887835473,
9.15590342972986));
#11074=CARTESIAN_POINT('Ctrl Pts',(0.822261614921547,-0.721264636910472,
9.1776904595879));
#11075=CARTESIAN_POINT('Ctrl Pts',(1.03025713637287,-0.238612529479814,
9.199437337924));
#11076=CARTESIAN_POINT('Ctrl Pts',(1.05171274317535,0.284808676532102,9.22115764762888));
#11077=CARTESIAN_POINT('Ctrl Pts',(0.707499007137911,0.882392330252907,
9.24826137586986));
#11078=CARTESIAN_POINT('Ctrl Pts',(0.0503973500479551,1.08358547878404,
9.27529841784466));
#11079=CARTESIAN_POINT('Ctrl Pts',(-0.452565343899477,0.9471545860309,9.2968858692952));
#11080=CARTESIAN_POINT('Ctrl Pts',(-0.801496735835974,0.690347253274425,
9.31485263733184));
#11081=CARTESIAN_POINT('Ctrl Pts',(-1.03251942952317,0.266238466090755,
9.33458892725171));
#11082=CARTESIAN_POINT('Ctrl Pts',(-1.03204243532931,-0.259297874573609,
9.35608057654046));
#11083=CARTESIAN_POINT('Ctrl Pts',(-0.781296145011018,-0.720337835230956,
9.37753649325143));
#11084=CARTESIAN_POINT('Ctrl Pts',(-0.340960105513239,-1.00413521062253,
9.39895573092214));
#11085=CARTESIAN_POINT('Ctrl Pts',(0.18048440489374,-1.04344608683549,9.42033660154328));
#11086=CARTESIAN_POINT('Ctrl Pts',(0.542239509342812,-0.879875126181648,
9.43656964857728));
#11087=CARTESIAN_POINT('Ctrl Pts',(0.736445066942167,-0.70113509377245,
9.44767340469813));
#11088=CARTESIAN_POINT('Ctrl Pts',(0.856894738517867,-0.55435325618568,
9.45566431872803));
#11089=CARTESIAN_POINT('Ctrl Pts',(1.01096117719817,-0.257122260199454,
9.46963825282641));
#11090=CARTESIAN_POINT('Ctrl Pts',(1.03289239306723,0.135256216575748,9.48558750066562));
#11091=CARTESIAN_POINT('Ctrl Pts',(0.896311081511608,0.491323200624549,
9.50151009167922));
#11092=CARTESIAN_POINT('Ctrl Pts',(0.667724538317195,0.795974688107478,
9.51741707525718));
#11093=CARTESIAN_POINT('Ctrl Pts',(0.239306522759663,1.03291901978371,9.53727288403102));
#11094=CARTESIAN_POINT('Ctrl Pts',(-0.346296088438099,0.99979161701914,
9.56105101819272));
#11095=CARTESIAN_POINT('Ctrl Pts',(-0.82345191390219,0.661042061037232,
9.58478160219318));
#11096=CARTESIAN_POINT('Ctrl Pts',(-1.04683085355964,0.121359459090256,
9.60846407228079));
#11097=CARTESIAN_POINT('Ctrl Pts',(-0.94901887957637,-0.453248775549408,
9.6320986882585));
#11098=CARTESIAN_POINT('Ctrl Pts',(-0.561282561137808,-0.886881598782615,
9.65568536824822));
#11099=CARTESIAN_POINT('Ctrl Pts',(-0.00339911447116993,-1.0474281541931,
9.67922421242135));
#11100=CARTESIAN_POINT('Ctrl Pts',(0.553257143873196,-0.886885387621517,
9.7027152735699));
#11101=CARTESIAN_POINT('Ctrl Pts',(0.938395324818619,-0.455667215824606,
9.72615865946567));
#11102=CARTESIAN_POINT('Ctrl Pts',(1.03488266426865,0.113203951634057,9.74955449029365));
#11103=CARTESIAN_POINT('Ctrl Pts',(0.81437044505405,0.645134483473366,9.77290291527007));
#11104=CARTESIAN_POINT('Ctrl Pts',(0.345602036856306,0.977539014113442,
9.79620411104843));
#11105=CARTESIAN_POINT('Ctrl Pts',(-0.227009525616586,1.00952652784022,
9.81945827173785));
#11106=CARTESIAN_POINT('Ctrl Pts',(-0.727866299354974,0.732522380427292,
9.84266563594512));
#11107=CARTESIAN_POINT('Ctrl Pts',(-1.00402898230868,0.232497928985327,
9.86582641828462));
#11108=CARTESIAN_POINT('Ctrl Pts',(-0.971909096055521,-0.336665090315949,
9.8889409732355));
#11109=CARTESIAN_POINT('Ctrl Pts',(-0.642564620330116,-0.800621732870167,
9.91200940971414));
#11110=CARTESIAN_POINT('Ctrl Pts',(-0.117930823376944,-1.01775421835117,
9.93503245984089));
#11111=CARTESIAN_POINT('Ctrl Pts',(0.44070282986155,-0.92286732415585,9.95800952149167));
#11112=CARTESIAN_POINT('Ctrl Pts',(0.862306840760016,-0.545707449143151,
9.98094303612929));
#11113=CARTESIAN_POINT('Ctrl Pts',(0.966341550947047,-0.18465912338656,
9.99619919808942));
#11114=CARTESIAN_POINT('Ctrl Pts',(0.966365964358855,-0.00331008130675842,
10.0038249694641));
#11115=CARTESIAN_POINT('Ctrl Pts',(1.0224395231333,0.0031540044764207,7.20006622055264));
#11116=CARTESIAN_POINT('Ctrl Pts',(1.02241370724182,0.194920999938243,7.20813006933056));
#11117=CARTESIAN_POINT('Ctrl Pts',(0.912366886309143,0.576958392287561,
7.22427144136625));
#11118=CARTESIAN_POINT('Ctrl Pts',(0.466456717327568,0.975815803916186,
7.24852425219416));
#11119=CARTESIAN_POINT('Ctrl Pts',(-0.124217636317022,1.0761482596652,7.27281852486299));
#11120=CARTESIAN_POINT('Ctrl Pts',(-0.678781147637653,0.846597884923694,
7.29715370167105));
#11121=CARTESIAN_POINT('Ctrl Pts',(-1.0267885200925,0.356304901332808,7.32152945959023));
#11122=CARTESIAN_POINT('Ctrl Pts',(-1.0606890229609,-0.244950870661962,
7.34594534636892));
#11123=CARTESIAN_POINT('Ctrl Pts',(-0.769035493636253,-0.772955750304005,
7.3704009447994));
#11124=CARTESIAN_POINT('Ctrl Pts',(-0.240329864575481,-1.0653237085793,
7.39489579641338));
#11125=CARTESIAN_POINT('Ctrl Pts',(0.363839304010974,-1.03153783690531,
7.41942943142408));
#11126=CARTESIAN_POINT('Ctrl Pts',(0.858198998883183,-0.680943831755809,
7.44400135772063));
#11127=CARTESIAN_POINT('Ctrl Pts',(1.0906063677628,-0.120209327641914,7.46861106610192));
#11128=CARTESIAN_POINT('Ctrl Pts',(0.988919658857672,0.479131132259177,
7.49325801533902));
#11129=CARTESIAN_POINT('Ctrl Pts',(0.583314808696736,0.933183422390409,
7.51794166559975));
#11130=CARTESIAN_POINT('Ctrl Pts',(-0.00247975052802087,1.1020802294482,
7.54266141162343));
#11131=CARTESIAN_POINT('Ctrl Pts',(-0.589337810114969,0.933196369368626,
7.56741671884064));
#11132=CARTESIAN_POINT('Ctrl Pts',(-0.981531482742348,0.494164393687638,
7.59128867034107));
#11133=CARTESIAN_POINT('Ctrl Pts',(-1.09283525118144,-0.0570023695692098,
7.61427269700993));
#11134=CARTESIAN_POINT('Ctrl Pts',(-0.933642969752733,-0.573400485891667,
7.63636381653099));
#11135=CARTESIAN_POINT('Ctrl Pts',(-0.546444722767111,-0.95111688919212,
7.65848129757189));
#11136=CARTESIAN_POINT('Ctrl Pts',(-0.0249538254466607,-1.09833623866965,
7.68062474544456));
#11137=CARTESIAN_POINT('Ctrl Pts',(0.503244146713521,-0.977119473107213,
7.70279347292931));
#11138=CARTESIAN_POINT('Ctrl Pts',(0.979497658227209,-0.559085504295418,
7.72868549174814));
#11139=CARTESIAN_POINT('Ctrl Pts',(1.14865259980211,0.175228209374103,7.75831545469268));
#11140=CARTESIAN_POINT('Ctrl Pts',(0.770334243068627,0.828201516454482,
7.78799180006802));
#11141=CARTESIAN_POINT('Ctrl Pts',(0.18976680663554,1.0887805913742,7.8139934791502));
#11142=CARTESIAN_POINT('Ctrl Pts',(-0.354152161259447,1.04824937041078,
7.83630306607929));
#11143=CARTESIAN_POINT('Ctrl Pts',(-0.774821505581955,0.776301631566783,
7.85677186261233));
#11144=CARTESIAN_POINT('Ctrl Pts',(-1.01364810108653,0.395754395150175,
7.87539596090851));
#11145=CARTESIAN_POINT('Ctrl Pts',(-1.08917134999908,-0.00205304235367609,
7.89216907011948));
#11146=CARTESIAN_POINT('Ctrl Pts',(-1.01353540633159,-0.399628518798629,
7.90895346821961));
#11147=CARTESIAN_POINT('Ctrl Pts',(-0.727131996125876,-0.858432305737684,
7.93134780330843));
#11148=CARTESIAN_POINT('Ctrl Pts',(-0.0863637973312472,-1.16829644414184,
7.95936473371975));
#11149=CARTESIAN_POINT('Ctrl Pts',(0.732678237418673,-0.915943411696203,
7.99302779994513));
#11150=CARTESIAN_POINT('Ctrl Pts',(1.16109954417639,-0.173577431070782,
8.02672930691054));
#11151=CARTESIAN_POINT('Ctrl Pts',(0.970648308118703,0.663040508180315,
8.06046758095857));
#11152=CARTESIAN_POINT('Ctrl Pts',(0.260283477478894,1.14757073863936,8.09424060232552));
#11153=CARTESIAN_POINT('Ctrl Pts',(-0.494518330344157,1.03279226984595,
8.12428848091482));
#11154=CARTESIAN_POINT('Ctrl Pts',(-0.95478161188669,0.581876430066912,
8.15060205079116));
#11155=CARTESIAN_POINT('Ctrl Pts',(-1.11772856826109,0.0548873179080656,
8.17316849900046));
#11156=CARTESIAN_POINT('Ctrl Pts',(-1.00819355033569,-0.486661028909071,
8.19574690136803));
#11157=CARTESIAN_POINT('Ctrl Pts',(-0.653258105050941,-0.910215074380895,
8.21833809577143));
#11158=CARTESIAN_POINT('Ctrl Pts',(-0.267209331026347,-1.06136783567525,
8.23528758547523));
#11159=CARTESIAN_POINT('Ctrl Pts',(0.000873105475631335,-1.07790421719274,
8.24659249433198));
#11160=CARTESIAN_POINT('Ctrl Pts',(0.179526465106109,-1.06678600021225,
8.25412966597351));
#11161=CARTESIAN_POINT('Ctrl Pts',(0.441661152994394,-1.00025121357308,
8.26543678412909));
#11162=CARTESIAN_POINT('Ctrl Pts',(0.74897005908796,-0.806537047527932,
8.2805156563327));
#11163=CARTESIAN_POINT('Ctrl Pts',(1.07539940103965,-0.367786484198072,
8.30314183095587));
#11164=CARTESIAN_POINT('Ctrl Pts',(1.13073755868417,0.348336730332993,8.33143620802701));
#11165=CARTESIAN_POINT('Ctrl Pts',(0.590404903092466,1.0253443836268,8.3654006862316));
#11166=CARTESIAN_POINT('Ctrl Pts',(-0.191896495262822,1.14202728535317,
8.39654847127686));
#11167=CARTESIAN_POINT('Ctrl Pts',(-0.803630405103391,0.802689596644375,
8.42487470313664));
#11168=CARTESIAN_POINT('Ctrl Pts',(-1.10777223118505,0.252867678305614,
8.45037283391805));
#11169=CARTESIAN_POINT('Ctrl Pts',(-1.07264929230278,-0.375831789681131,
8.47587587326063));
#11170=CARTESIAN_POINT('Ctrl Pts',(-0.775756370582944,-0.793138595001687,
8.49665696129285));
#11171=CARTESIAN_POINT('Ctrl Pts',(-0.370973206955298,-1.04054893447855,
8.51649811440533));
#11172=CARTESIAN_POINT('Ctrl Pts',(0.038369462981197,-1.11292368936976,
8.53350571642248));
#11173=CARTESIAN_POINT('Ctrl Pts',(0.47898976689409,-0.994340382144285,
8.55240171155723));
#11174=CARTESIAN_POINT('Ctrl Pts',(0.80923417022507,-0.750922678629335,
8.56941016515415));
#11175=CARTESIAN_POINT('Ctrl Pts',(1.0274182871984,-0.403326067555486,8.58641602817986));
#11176=CARTESIAN_POINT('Ctrl Pts',(1.11691118054261,0.0671129407531136,
8.60625737788999));
#11177=CARTESIAN_POINT('Ctrl Pts',(0.962508000998029,0.604452525770246,
8.62892861065794));
#11178=CARTESIAN_POINT('Ctrl Pts',(0.493205548534116,1.02369118998224,8.65443255406071));
#11179=CARTESIAN_POINT('Ctrl Pts',(-0.126835973873531,1.12902274781952,
8.67993208193622));
#11180=CARTESIAN_POINT('Ctrl Pts',(-0.707895425994039,0.888341330697344,
8.70542701256162));
#11181=CARTESIAN_POINT('Ctrl Pts',(-1.07169802862448,0.375537140185558,
8.73091586806527));
#11182=CARTESIAN_POINT('Ctrl Pts',(-1.10692322919911,-0.252055003610382,
8.75639778158459));
#11183=CARTESIAN_POINT('Ctrl Pts',(-0.802931792932112,-0.802016307091765,
8.7818716346359));
#11184=CARTESIAN_POINT('Ctrl Pts',(-0.253135892745948,-1.10583889227955,
8.80733643557024));
#11185=CARTESIAN_POINT('Ctrl Pts',(0.373787124048757,-1.07059371077824,
8.83279114625073));
#11186=CARTESIAN_POINT('Ctrl Pts',(0.885644972309457,-0.707362970666774,
8.85823476032552));
#11187=CARTESIAN_POINT('Ctrl Pts',(1.1256782624904,-0.127754861211958,8.88366627230367));
#11188=CARTESIAN_POINT('Ctrl Pts',(1.02061722935054,0.490400628571495,8.90908465879932));
#11189=CARTESIAN_POINT('Ctrl Pts',(0.602991135209833,0.957653872010445,
8.93448895110668));
#11190=CARTESIAN_POINT('Ctrl Pts',(0.00120859626939015,1.13099126811469,
8.95987805769087));
#11191=CARTESIAN_POINT('Ctrl Pts',(-0.600287978023236,0.957707910761615,
8.98525114960464));
#11192=CARTESIAN_POINT('Ctrl Pts',(-1.00136692422523,0.508544235532217,
9.00966765026286));
#11193=CARTESIAN_POINT('Ctrl Pts',(-1.11475583894706,-0.0541766995265247,
9.03312999675204));
#11194=CARTESIAN_POINT('Ctrl Pts',(-0.952788419669591,-0.580292773132626,
9.05564117304827));
#11195=CARTESIAN_POINT('Ctrl Pts',(-0.591528141422974,-0.932614863756553,
9.07626128741052));
#11196=CARTESIAN_POINT('Ctrl Pts',(-0.164923344909653,-1.0810596235015,
9.0949942575564));
#11197=CARTESIAN_POINT('Ctrl Pts',(0.377658114142277,-1.06225637331858,
9.11746360413473));
#11198=CARTESIAN_POINT('Ctrl Pts',(0.848868791300341,-0.74246439931946,
9.13990987964604));
#11199=CARTESIAN_POINT('Ctrl Pts',(1.06344806548654,-0.244595576832108,
9.162338498867));
#11200=CARTESIAN_POINT('Ctrl Pts',(1.08562630996489,0.295649655289467,9.18475421262983));
#11201=CARTESIAN_POINT('Ctrl Pts',(0.730193182157616,0.912995733937815,
9.21274171873496));
#11202=CARTESIAN_POINT('Ctrl Pts',(0.0507146947130891,1.12120769041665,
9.24069241304767));
#11203=CARTESIAN_POINT('Ctrl Pts',(-0.469908160478353,0.98001973592613,
9.26303328476729));
#11204=CARTESIAN_POINT('Ctrl Pts',(-0.831281954576518,0.714080478677811,
9.28163790668312));
#11205=CARTESIAN_POINT('Ctrl Pts',(-1.0707247835365,0.274656717484436,9.30208197073574));
#11206=CARTESIAN_POINT('Ctrl Pts',(-1.07026628651612,-0.270334760718956,
9.32436700779422));
#11207=CARTESIAN_POINT('Ctrl Pts',(-0.81012944245468,-0.748778183184174,
9.34662760904691));
#11208=CARTESIAN_POINT('Ctrl Pts',(-0.352913623587519,-1.04349781871771,
9.36886459486743));
#11209=CARTESIAN_POINT('Ctrl Pts',(0.18892490073276,-1.08440077143083,9.39108033469003));
#11210=CARTESIAN_POINT('Ctrl Pts',(0.565010389578148,-0.914360468661282,
9.40794963584902));
#11211=CARTESIAN_POINT('Ctrl Pts',(0.767035294725711,-0.728425442708479,
9.41949991154068));
#11212=CARTESIAN_POINT('Ctrl Pts',(0.892355216546134,-0.575710200559469,
9.42781320640248));
#11213=CARTESIAN_POINT('Ctrl Pts',(1.05269478111425,-0.266393255154064,
9.44235418619472));
#11214=CARTESIAN_POINT('Ctrl Pts',(1.07555876507525,0.142080540702115,9.45895154635578));
#11215=CARTESIAN_POINT('Ctrl Pts',(0.933282910553863,0.513021814758867,
9.47553758890735));
#11216=CARTESIAN_POINT('Ctrl Pts',(0.695081061939374,0.830497822734072,
9.49211211559699));
#11217=CARTESIAN_POINT('Ctrl Pts',(0.248476724545638,1.07754915938558,9.51280614214995));
#11218=CARTESIAN_POINT('Ctrl Pts',(-0.362433114682866,1.04304224887823,
9.53760669954168));
#11219=CARTESIAN_POINT('Ctrl Pts',(-0.860534362744572,0.689473898600431,
9.56237202551932));
#11220=CARTESIAN_POINT('Ctrl Pts',(-1.09388928914477,0.125810273797895,
9.58710240698908));
#11221=CARTESIAN_POINT('Ctrl Pts',(-0.991713095702174,-0.474700208975981,
9.61179677753925));
#11222=CARTESIAN_POINT('Ctrl Pts',(-0.586315730889703,-0.928151038584933,
9.63645472421636));
#11223=CARTESIAN_POINT('Ctrl Pts',(-0.00268034821758927,-1.09615308592063,
9.66107559259117));
#11224=CARTESIAN_POINT('Ctrl Pts',(0.579985073663781,-0.928151554047772,
9.68565886740576));
#11225=CARTESIAN_POINT('Ctrl Pts',(0.983331340832418,-0.476604367726687,
9.71020401270546));
#11226=CARTESIAN_POINT('Ctrl Pts',(1.08445410902017,0.119383118454789,9.73471053368719));
#11227=CARTESIAN_POINT('Ctrl Pts',(0.85335961648174,0.676927075373189,9.75917795165438));
#11228=CARTESIAN_POINT('Ctrl Pts',(0.361848605557405,1.02549620846588,9.78360581484665));
#11229=CARTESIAN_POINT('Ctrl Pts',(-0.238792954238506,1.05907901718415,
9.80799368150402));
#11230=CARTESIAN_POINT('Ctrl Pts',(-0.764369402329827,0.768436104225106,
9.83234115979546));
#11231=CARTESIAN_POINT('Ctrl Pts',(-1.05427545134513,0.243589360885239,
9.85664781917723));
#11232=CARTESIAN_POINT('Ctrl Pts',(-1.02057935151888,-0.354025448888461,
9.88091336937157));
#11233=CARTESIAN_POINT('Ctrl Pts',(-0.674705848488251,-0.841316796753126,
9.90513727965942));
#11234=CARTESIAN_POINT('Ctrl Pts',(-0.123577927191511,-1.06944251069366,
9.92931960214379));
#11235=CARTESIAN_POINT('Ctrl Pts',(0.46338865969666,-0.969738708423244,
9.95345913840996));
#11236=CARTESIAN_POINT('Ctrl Pts',(0.906472097123054,-0.573379692131889,
9.97755753026823));
#11237=CARTESIAN_POINT('Ctrl Pts',(1.01577492904176,-0.193792191488556,
9.99359268772338));
#11238=CARTESIAN_POINT('Ctrl Pts',(1.01580058362196,-0.00322343436719488,
10.0016061503604));
#11239=CARTESIAN_POINT('Ctrl Pts',(0.999999575810999,0.00315098358513781,
7.20006622055264));
#11240=CARTESIAN_POINT('Ctrl Pts',(0.999974319608277,0.190760468856422,
7.20795524501636));
#11241=CARTESIAN_POINT('Ctrl Pts',(0.892344234443071,0.564401735476683,
7.22374165130483));
#11242=CARTESIAN_POINT('Ctrl Pts',(0.456170863303355,0.954569139239392,
7.24746551842362));
#11243=CARTESIAN_POINT('Ctrl Pts',(-0.121643296695006,1.0527111229517,7.27123039275792));
#11244=CARTESIAN_POINT('Ctrl Pts',(-0.664174499114347,0.828146653873478,
7.29503750827097));
#11245=CARTESIAN_POINT('Ctrl Pts',(-1.00466229107333,0.348451955041142,
7.31888617441183));
#11246=CARTESIAN_POINT('Ctrl Pts',(-1.03783821085617,-0.239862803165599,
7.34277653444097));
#11247=CARTESIAN_POINT('Ctrl Pts',(-0.752436914310739,-0.756562482852077,
7.36670833282365));
#11248=CARTESIAN_POINT('Ctrl Pts',(-0.234997931414651,-1.04270891419437,
7.39068146490982));
#11249=CARTESIAN_POINT('Ctrl Pts',(0.356377432582172,-1.00964746384867,
7.41469572763747));
#11250=CARTESIAN_POINT('Ctrl Pts',(0.840341677037224,-0.666437865062604,
7.43875093208249));
#11251=CARTESIAN_POINT('Ctrl Pts',(1.06790358406505,-0.117422164195028,
7.4628468515188));
#11252=CARTESIAN_POINT('Ctrl Pts',(0.968336509361683,0.469494166098508,
7.48698324256581));
#11253=CARTESIAN_POINT('Ctrl Pts',(0.571081336399399,0.914217869413367,
7.51115983904362));
#11254=CARTESIAN_POINT('Ctrl Pts',(-0.00276942901145937,1.07968430615977,
7.53537635143244));
#11255=CARTESIAN_POINT('Ctrl Pts',(-0.577781503135752,0.914223804149117,
7.55963247041146));
#11256=CARTESIAN_POINT('Ctrl Pts',(-0.962145622562424,0.483976677731404,
7.58302803095162));
#11257=CARTESIAN_POINT('Ctrl Pts',(-1.07125753086067,-0.0562794445165808,
7.60555779623404));
#11258=CARTESIAN_POINT('Ctrl Pts',(-0.915194862614763,-0.562561634031091,
7.6272168563822));
#11259=CARTESIAN_POINT('Ctrl Pts',(-0.53551487530705,-0.932963762094015,
7.64890612590553));
#11260=CARTESIAN_POINT('Ctrl Pts',(-0.024035065806305,-1.07736876663697,
7.67062531437742));
#11261=CARTESIAN_POINT('Ctrl Pts',(0.494146757015346,-0.958466814289234,
7.69237411680017));
#11262=CARTESIAN_POINT('Ctrl Pts',(0.961479539986573,-0.548279772601945,
7.71778190065853));
#11263=CARTESIAN_POINT('Ctrl Pts',(1.12756301652098,0.172482400610549,7.74686765103336));
#11264=CARTESIAN_POINT('Ctrl Pts',(0.75611713355168,0.813684959589575,7.77601030696451));
#11265=CARTESIAN_POINT('Ctrl Pts',(0.185875815215743,1.06965010757807,7.80155082448588));
#11266=CARTESIAN_POINT('Ctrl Pts',(-0.348517058347165,1.02984652160674,
7.82347022110603));
#11267=CARTESIAN_POINT('Ctrl Pts',(-0.761949296282463,0.762592777124389,
7.84358787235736));
#11268=CARTESIAN_POINT('Ctrl Pts',(-0.996722963062006,0.388518849169714,
7.86189613571743));
#11269=CARTESIAN_POINT('Ctrl Pts',(-1.07098690831041,-0.00260829917091459,
7.87838843437341));
#11270=CARTESIAN_POINT('Ctrl Pts',(-0.99661183226746,-0.393594984460838,
7.894895410549));
#11271=CARTESIAN_POINT('Ctrl Pts',(-0.714908576434247,-0.844892296878379,
7.9169240469514));
#11272=CARTESIAN_POINT('Ctrl Pts',(-0.084422651145012,-1.14985023564212,
7.94449562780488));
#11273=CARTESIAN_POINT('Ctrl Pts',(0.721887320494981,-0.901498071462995,
7.97763725360595));
#11274=CARTESIAN_POINT('Ctrl Pts',(1.14390600676876,-0.170383526932712,
8.01083302661308));
#11275=CARTESIAN_POINT('Ctrl Pts',(0.956311918053777,0.65401391794098,8.04408130906187));
#11276=CARTESIAN_POINT('Ctrl Pts',(0.25602906697655,1.13176193513965,8.07738040653961));
#11277=CARTESIAN_POINT('Ctrl Pts',(-0.488510543500641,1.01860423556296,
8.10702323570327));
#11278=CARTESIAN_POINT('Ctrl Pts',(-0.942716248260153,0.573655629467007,
8.13299136011509));
#11279=CARTESIAN_POINT('Ctrl Pts',(-1.10358636285334,0.0534364176198665,
8.15527022722507));
#11280=CARTESIAN_POINT('Ctrl Pts',(-0.99543872479676,-0.481361877750802,
8.17756901902506));
#11281=CARTESIAN_POINT('Ctrl Pts',(-0.644826641417894,-0.899786909633448,
8.1998871769012));
#11282=CARTESIAN_POINT('Ctrl Pts',(-0.263312902512338,-1.04918995788175,
8.21663989380025));
#11283=CARTESIAN_POINT('Ctrl Pts',(0.00166665731618679,-1.0655343402046,
8.22781406534667));
#11284=CARTESIAN_POINT('Ctrl Pts',(0.178270288589001,-1.05454413855026,
8.23526501957515));
#11285=CARTESIAN_POINT('Ctrl Pts',(0.437439999691742,-0.98876491629653,
8.24644481283225));
#11286=CARTESIAN_POINT('Ctrl Pts',(0.741357296669408,-0.797196125183601,
8.26135855011107));
#11287=CARTESIAN_POINT('Ctrl Pts',(1.06427742047819,-0.363196133741635,
8.28374205636937));
#11288=CARTESIAN_POINT('Ctrl Pts',(1.1191132547847,0.345488423812591,8.31174498186711));
#11289=CARTESIAN_POINT('Ctrl Pts',(0.584140656179565,1.01596202851522,8.34538413710338));
#11290=CARTESIAN_POINT('Ctrl Pts',(-0.19096844855633,1.13165287559935,8.37625078730322));
#11291=CARTESIAN_POINT('Ctrl Pts',(-0.797411359462935,0.795301993540907,
8.40433431031039));
#11292=CARTESIAN_POINT('Ctrl Pts',(-1.0990783559073,0.250015446968417,8.4296262708737));
#11293=CARTESIAN_POINT('Ctrl Pts',(-1.06426569125542,-0.373802040240765,
8.45493410201599));
#11294=CARTESIAN_POINT('Ctrl Pts',(-0.769553388901587,-0.788092512102153,
8.47556748693345));
#11295=CARTESIAN_POINT('Ctrl Pts',(-0.367608264833719,-1.03377453912702,
8.49527086803642));
#11296=CARTESIAN_POINT('Ctrl Pts',(0.0389894662197936,-1.10568483145998,
8.51216552927169));
#11297=CARTESIAN_POINT('Ctrl Pts',(0.476842798425807,-0.987859734068039,
8.53094473644388));
#11298=CARTESIAN_POINT('Ctrl Pts',(0.805101130351003,-0.7459169684144,8.54785141982868));
#11299=CARTESIAN_POINT('Ctrl Pts',(1.02206224073455,-0.400294829517718,
8.56476322077897));
#11300=CARTESIAN_POINT('Ctrl Pts',(1.11108597940432,0.0676090739442989,
8.58449929513004));
#11301=CARTESIAN_POINT('Ctrl Pts',(0.957486327179168,0.602305552598091,
8.60706239241156));
#11302=CARTESIAN_POINT('Ctrl Pts',(0.490319176226327,1.0196961225561,8.63245514939238));
#11303=CARTESIAN_POINT('Ctrl Pts',(-0.127227772869885,1.12465246691674,
8.65785621578684));
#11304=CARTESIAN_POINT('Ctrl Pts',(-0.706252354762176,0.884861784560879,
8.6832646175365));
#11305=CARTESIAN_POINT('Ctrl Pts',(-1.06898139570907,0.373646110671472,
8.70867937640931));
#11306=CARTESIAN_POINT('Ctrl Pts',(-1.10415883703196,-0.252336062683339,
8.73409951326223));
#11307=CARTESIAN_POINT('Ctrl Pts',(-0.800834752831557,-0.801177522527246,
8.75952404569165));
#11308=CARTESIAN_POINT('Ctrl Pts',(-0.251930241323733,-1.10455619700772,
8.78495198825788));
#11309=CARTESIAN_POINT('Ctrl Pts',(0.374309533721303,-1.06939244573458,
8.81038235029736));
#11310=CARTESIAN_POINT('Ctrl Pts',(0.88588373813812,-0.706416051605379,
8.83581414648952));
#11311=CARTESIAN_POINT('Ctrl Pts',(1.12593002076033,-0.126889341474946,
8.86124638643539));
#11312=CARTESIAN_POINT('Ctrl Pts',(1.02087104515559,0.491507891337351,8.88667807898767));
#11313=CARTESIAN_POINT('Ctrl Pts',(0.602911335681679,0.959196578831539,
8.91210823370906));
#11314=CARTESIAN_POINT('Ctrl Pts',(0.000316973456126708,1.13280882473463,
8.93753586563178));
#11315=CARTESIAN_POINT('Ctrl Pts',(-0.602311983560242,0.959240722445107,
8.9629599838141));
#11316=CARTESIAN_POINT('Ctrl Pts',(-1.00436822137552,0.509038661422071,
8.98743813657581));
#11317=CARTESIAN_POINT('Ctrl Pts',(-1.11811011681427,-0.0552669144060651,
9.01097002817133));
#11318=CARTESIAN_POINT('Ctrl Pts',(-0.955644771077333,-0.583087731975911,
9.03355562561233));
#11319=CARTESIAN_POINT('Ctrl Pts',(-0.593074356957321,-0.936728146430118,
9.0542538609391));
#11320=CARTESIAN_POINT('Ctrl Pts',(-0.164731041598437,-1.08578943530602,
9.07306578079699));
#11321=CARTESIAN_POINT('Ctrl Pts',(0.380219776536112,-1.06693040182505,
9.09563491033651));
#11322=CARTESIAN_POINT('Ctrl Pts',(0.853779549938941,-0.745621203287222,
9.11819570154211));
#11323=CARTESIAN_POINT('Ctrl Pts',(1.06953462325323,-0.245092836305948,
9.14074702398398));
#11324=CARTESIAN_POINT('Ctrl Pts',(1.09185195352203,0.298202592837182,9.16329164905568));
#11325=CARTESIAN_POINT('Ctrl Pts',(0.734297058725123,0.919425032182445,
9.19145918094331));
#11326=CARTESIAN_POINT('Ctrl Pts',(0.0501860572080287,1.12913650428628,
9.21960716991184));
#11327=CARTESIAN_POINT('Ctrl Pts',(-0.47422284767955,0.986938013732599,
9.24211273100823));
#11328=CARTESIAN_POINT('Ctrl Pts',(-0.83834294439581,0.718994011703782,
9.26085993499593));
#11329=CARTESIAN_POINT('Ctrl Pts',(-1.0797140885543,0.276058653254629,9.28147192866405));
#11330=CARTESIAN_POINT('Ctrl Pts',(-1.0792869722179,-0.273490761429736,
9.30394472055128));
#11331=CARTESIAN_POINT('Ctrl Pts',(-0.816874083948392,-0.756154521252702,
9.32640385818033));
#11332=CARTESIAN_POINT('Ctrl Pts',(-0.355458797527567,-1.05362205517351,
9.34884870640624));
#11333=CARTESIAN_POINT('Ctrl Pts',(0.191577194376755,-1.09493860698716,
9.37127864639074));
#11334=CARTESIAN_POINT('Ctrl Pts',(0.571484722667441,-0.923210767165354,
9.38832293897591));
#11335=CARTESIAN_POINT('Ctrl Pts',(0.775578610165073,-0.735373724461368,
9.39999172743641));
#11336=CARTESIAN_POINT('Ctrl Pts',(0.90219668945127,-0.581077610283799,
9.40839153478326));
#11337=CARTESIAN_POINT('Ctrl Pts',(1.06423218001646,-0.268505675241936,
9.42308663622534));
#11338=CARTESIAN_POINT('Ctrl Pts',(1.08737574685665,0.14445700622961,9.43987039483926));
#11339=CARTESIAN_POINT('Ctrl Pts',(0.943512119332504,0.519555849049532,
9.45664308969273));
#11340=CARTESIAN_POINT('Ctrl Pts',(0.702595952885493,0.840663912121189,
9.47340826939813));
#11341=CARTESIAN_POINT('Ctrl Pts',(0.250731034525726,1.09066378632527,9.49435038976507));
#11342=CARTESIAN_POINT('Ctrl Pts',(-0.367646366337481,1.05577469318307,
9.51945715090945));
#11343=CARTESIAN_POINT('Ctrl Pts',(-0.872073427555176,0.697769149747224,
9.54453931621249));
#11344=CARTESIAN_POINT('Ctrl Pts',(-1.10851395153864,0.126754498956172,
9.56959609551394));
#11345=CARTESIAN_POINT('Ctrl Pts',(-1.004997965557,-0.481859237919703,9.59462670660628));
#11346=CARTESIAN_POINT('Ctrl Pts',(-0.593994937248818,-0.94163509404227,
9.61963038098806));
#11347=CARTESIAN_POINT('Ctrl Pts',(-0.0020235655980388,-1.11207375119343,
9.6446063758667));
#11348=CARTESIAN_POINT('Ctrl Pts',(0.589215999041395,-0.941636436533483,
9.66955394755264));
#11349=CARTESIAN_POINT('Ctrl Pts',(0.99867475328867,-0.483298149068583,
9.69447238340543));
#11350=CARTESIAN_POINT('Ctrl Pts',(1.10139617547556,0.121906639873499,9.71936097538517));
#11351=CARTESIAN_POINT('Ctrl Pts',(0.866669607038716,0.688301956936916,
9.74421904187644));
#11352=CARTESIAN_POINT('Ctrl Pts',(0.367204775824758,1.0425526426198,9.76904590972932));
#11353=CARTESIAN_POINT('Ctrl Pts',(-0.243395435261487,1.07672488055471,
9.79384092765142));
#11354=CARTESIAN_POINT('Ctrl Pts',(-0.777888567237211,0.781186417289152,
9.81860345995005));
#11355=CARTESIAN_POINT('Ctrl Pts',(-1.07283036518199,0.247282943918733,
9.84333289822209));
#11356=CARTESIAN_POINT('Ctrl Pts',(-1.03856704754786,-0.360866232625645,
9.86802861303319));
#11357=CARTESIAN_POINT('Ctrl Pts',(-0.686501281653619,-0.856920605922548,
9.892690097101));
#11358=CARTESIAN_POINT('Ctrl Pts',(-0.125304938207573,-1.08924443021579,
9.91731661435472));
#11359=CARTESIAN_POINT('Ctrl Pts',(0.472593334675849,-0.987703022851267,
9.94190800522239));
#11360=CARTESIAN_POINT('Ctrl Pts',(0.924078607982629,-0.583894056083662,
9.9664628819065));
#11361=CARTESIAN_POINT('Ctrl Pts',(1.03553205098759,-0.196980695813872,
9.98281022139497));
#11362=CARTESIAN_POINT('Ctrl Pts',(1.03555819462295,-0.00277911247133682,
9.99097644525911));
#11363=CARTESIAN_POINT('',(0.999999575810999,0.00315098358513782,7.20006622055264));
#11364=CARTESIAN_POINT('Origin',(1.,0.,7.275));
#11365=CARTESIAN_POINT('',(1.03555819462295,-0.00277911247133681,9.99097644525911));
#11366=CARTESIAN_POINT('Ctrl Pts',(0.999999575810999,0.00315098358513781,
7.20006622055264));
#11367=CARTESIAN_POINT('Ctrl Pts',(0.999974319608277,0.190760468856422,
7.20795524501636));
#11368=CARTESIAN_POINT('Ctrl Pts',(0.892344234443071,0.564401735476683,
7.22374165130483));
#11369=CARTESIAN_POINT('Ctrl Pts',(0.456170863303355,0.954569139239392,
7.24746551842362));
#11370=CARTESIAN_POINT('Ctrl Pts',(-0.121643296695006,1.0527111229517,7.27123039275792));
#11371=CARTESIAN_POINT('Ctrl Pts',(-0.664174499114347,0.828146653873478,
7.29503750827097));
#11372=CARTESIAN_POINT('Ctrl Pts',(-1.00466229107333,0.348451955041142,
7.31888617441183));
#11373=CARTESIAN_POINT('Ctrl Pts',(-1.03783821085617,-0.239862803165599,
7.34277653444097));
#11374=CARTESIAN_POINT('Ctrl Pts',(-0.752436914310739,-0.756562482852077,
7.36670833282365));
#11375=CARTESIAN_POINT('Ctrl Pts',(-0.234997931414651,-1.04270891419437,
7.39068146490982));
#11376=CARTESIAN_POINT('Ctrl Pts',(0.356377432582172,-1.00964746384867,
7.41469572763747));
#11377=CARTESIAN_POINT('Ctrl Pts',(0.840341677037224,-0.666437865062604,
7.43875093208249));
#11378=CARTESIAN_POINT('Ctrl Pts',(1.06790358406505,-0.117422164195028,
7.4628468515188));
#11379=CARTESIAN_POINT('Ctrl Pts',(0.968336509361683,0.469494166098508,
7.48698324256581));
#11380=CARTESIAN_POINT('Ctrl Pts',(0.571081336399399,0.914217869413367,
7.51115983904362));
#11381=CARTESIAN_POINT('Ctrl Pts',(-0.00276942901145937,1.07968430615977,
7.53537635143244));
#11382=CARTESIAN_POINT('Ctrl Pts',(-0.577781503135752,0.914223804149117,
7.55963247041146));
#11383=CARTESIAN_POINT('Ctrl Pts',(-0.962145622562424,0.483976677731404,
7.58302803095162));
#11384=CARTESIAN_POINT('Ctrl Pts',(-1.07125753086067,-0.0562794445165808,
7.60555779623404));
#11385=CARTESIAN_POINT('Ctrl Pts',(-0.915194862614763,-0.562561634031091,
7.6272168563822));
#11386=CARTESIAN_POINT('Ctrl Pts',(-0.53551487530705,-0.932963762094015,
7.64890612590553));
#11387=CARTESIAN_POINT('Ctrl Pts',(-0.024035065806305,-1.07736876663697,
7.67062531437742));
#11388=CARTESIAN_POINT('Ctrl Pts',(0.494146757015346,-0.958466814289234,
7.69237411680017));
#11389=CARTESIAN_POINT('Ctrl Pts',(0.961479539986573,-0.548279772601945,
7.71778190065853));
#11390=CARTESIAN_POINT('Ctrl Pts',(1.12756301652098,0.172482400610549,7.74686765103336));
#11391=CARTESIAN_POINT('Ctrl Pts',(0.75611713355168,0.813684959589575,7.77601030696451));
#11392=CARTESIAN_POINT('Ctrl Pts',(0.185875815215743,1.06965010757807,7.80155082448588));
#11393=CARTESIAN_POINT('Ctrl Pts',(-0.348517058347165,1.02984652160674,
7.82347022110603));
#11394=CARTESIAN_POINT('Ctrl Pts',(-0.761949296282463,0.762592777124389,
7.84358787235736));
#11395=CARTESIAN_POINT('Ctrl Pts',(-0.996722963062006,0.388518849169714,
7.86189613571743));
#11396=CARTESIAN_POINT('Ctrl Pts',(-1.07098690831041,-0.00260829917091459,
7.87838843437341));
#11397=CARTESIAN_POINT('Ctrl Pts',(-0.99661183226746,-0.393594984460838,
7.894895410549));
#11398=CARTESIAN_POINT('Ctrl Pts',(-0.714908576434247,-0.844892296878379,
7.9169240469514));
#11399=CARTESIAN_POINT('Ctrl Pts',(-0.084422651145012,-1.14985023564212,
7.94449562780488));
#11400=CARTESIAN_POINT('Ctrl Pts',(0.721887320494981,-0.901498071462995,
7.97763725360595));
#11401=CARTESIAN_POINT('Ctrl Pts',(1.14390600676876,-0.170383526932712,
8.01083302661308));
#11402=CARTESIAN_POINT('Ctrl Pts',(0.956311918053777,0.65401391794098,8.04408130906187));
#11403=CARTESIAN_POINT('Ctrl Pts',(0.25602906697655,1.13176193513965,8.07738040653961));
#11404=CARTESIAN_POINT('Ctrl Pts',(-0.488510543500641,1.01860423556296,
8.10702323570327));
#11405=CARTESIAN_POINT('Ctrl Pts',(-0.942716248260153,0.573655629467007,
8.13299136011509));
#11406=CARTESIAN_POINT('Ctrl Pts',(-1.10358636285334,0.0534364176198665,
8.15527022722507));
#11407=CARTESIAN_POINT('Ctrl Pts',(-0.99543872479676,-0.481361877750802,
8.17756901902506));
#11408=CARTESIAN_POINT('Ctrl Pts',(-0.644826641417894,-0.899786909633448,
8.1998871769012));
#11409=CARTESIAN_POINT('Ctrl Pts',(-0.263312902512338,-1.04918995788175,
8.21663989380025));
#11410=CARTESIAN_POINT('Ctrl Pts',(0.00166665731618679,-1.0655343402046,
8.22781406534667));
#11411=CARTESIAN_POINT('Ctrl Pts',(0.178270288589001,-1.05454413855026,
8.23526501957515));
#11412=CARTESIAN_POINT('Ctrl Pts',(0.437439999691742,-0.98876491629653,
8.24644481283225));
#11413=CARTESIAN_POINT('Ctrl Pts',(0.741357296669408,-0.797196125183601,
8.26135855011107));
#11414=CARTESIAN_POINT('Ctrl Pts',(1.06427742047819,-0.363196133741635,
8.28374205636937));
#11415=CARTESIAN_POINT('Ctrl Pts',(1.1191132547847,0.345488423812591,8.31174498186711));
#11416=CARTESIAN_POINT('Ctrl Pts',(0.584140656179565,1.01596202851522,8.34538413710338));
#11417=CARTESIAN_POINT('Ctrl Pts',(-0.19096844855633,1.13165287559935,8.37625078730322));
#11418=CARTESIAN_POINT('Ctrl Pts',(-0.797411359462935,0.795301993540907,
8.40433431031039));
#11419=CARTESIAN_POINT('Ctrl Pts',(-1.0990783559073,0.250015446968417,8.4296262708737));
#11420=CARTESIAN_POINT('Ctrl Pts',(-1.06426569125542,-0.373802040240765,
8.45493410201599));
#11421=CARTESIAN_POINT('Ctrl Pts',(-0.769553388901587,-0.788092512102153,
8.47556748693345));
#11422=CARTESIAN_POINT('Ctrl Pts',(-0.367608264833719,-1.03377453912702,
8.49527086803642));
#11423=CARTESIAN_POINT('Ctrl Pts',(0.0389894662197936,-1.10568483145998,
8.51216552927169));
#11424=CARTESIAN_POINT('Ctrl Pts',(0.476842798425807,-0.987859734068039,
8.53094473644388));
#11425=CARTESIAN_POINT('Ctrl Pts',(0.805101130351003,-0.7459169684144,8.54785141982868));
#11426=CARTESIAN_POINT('Ctrl Pts',(1.02206224073455,-0.400294829517718,
8.56476322077897));
#11427=CARTESIAN_POINT('Ctrl Pts',(1.11108597940432,0.0676090739442989,
8.58449929513004));
#11428=CARTESIAN_POINT('Ctrl Pts',(0.957486327179168,0.602305552598091,
8.60706239241156));
#11429=CARTESIAN_POINT('Ctrl Pts',(0.490319176226327,1.0196961225561,8.63245514939238));
#11430=CARTESIAN_POINT('Ctrl Pts',(-0.127227772869885,1.12465246691674,
8.65785621578684));
#11431=CARTESIAN_POINT('Ctrl Pts',(-0.706252354762176,0.884861784560879,
8.6832646175365));
#11432=CARTESIAN_POINT('Ctrl Pts',(-1.06898139570907,0.373646110671472,
8.70867937640931));
#11433=CARTESIAN_POINT('Ctrl Pts',(-1.10415883703196,-0.252336062683339,
8.73409951326223));
#11434=CARTESIAN_POINT('Ctrl Pts',(-0.800834752831557,-0.801177522527246,
8.75952404569165));
#11435=CARTESIAN_POINT('Ctrl Pts',(-0.251930241323733,-1.10455619700772,
8.78495198825788));
#11436=CARTESIAN_POINT('Ctrl Pts',(0.374309533721303,-1.06939244573458,
8.81038235029736));
#11437=CARTESIAN_POINT('Ctrl Pts',(0.88588373813812,-0.706416051605379,
8.83581414648952));
#11438=CARTESIAN_POINT('Ctrl Pts',(1.12593002076033,-0.126889341474946,
8.86124638643539));
#11439=CARTESIAN_POINT('Ctrl Pts',(1.02087104515559,0.491507891337351,8.88667807898767));
#11440=CARTESIAN_POINT('Ctrl Pts',(0.602911335681679,0.959196578831539,
8.91210823370906));
#11441=CARTESIAN_POINT('Ctrl Pts',(0.000316973456126708,1.13280882473463,
8.93753586563178));
#11442=CARTESIAN_POINT('Ctrl Pts',(-0.602311983560242,0.959240722445107,
8.9629599838141));
#11443=CARTESIAN_POINT('Ctrl Pts',(-1.00436822137552,0.509038661422071,
8.98743813657581));
#11444=CARTESIAN_POINT('Ctrl Pts',(-1.11811011681427,-0.0552669144060651,
9.01097002817133));
#11445=CARTESIAN_POINT('Ctrl Pts',(-0.955644771077333,-0.583087731975911,
9.03355562561233));
#11446=CARTESIAN_POINT('Ctrl Pts',(-0.593074356957321,-0.936728146430118,
9.0542538609391));
#11447=CARTESIAN_POINT('Ctrl Pts',(-0.164731041598437,-1.08578943530602,
9.07306578079699));
#11448=CARTESIAN_POINT('Ctrl Pts',(0.380219776536112,-1.06693040182505,
9.09563491033651));
#11449=CARTESIAN_POINT('Ctrl Pts',(0.853779549938941,-0.745621203287222,
9.11819570154211));
#11450=CARTESIAN_POINT('Ctrl Pts',(1.06953462325323,-0.245092836305948,
9.14074702398398));
#11451=CARTESIAN_POINT('Ctrl Pts',(1.09185195352203,0.298202592837182,9.16329164905568));
#11452=CARTESIAN_POINT('Ctrl Pts',(0.734297058725123,0.919425032182445,
9.19145918094331));
#11453=CARTESIAN_POINT('Ctrl Pts',(0.0501860572080287,1.12913650428628,
9.21960716991184));
#11454=CARTESIAN_POINT('Ctrl Pts',(-0.47422284767955,0.986938013732599,
9.24211273100823));
#11455=CARTESIAN_POINT('Ctrl Pts',(-0.83834294439581,0.718994011703782,
9.26085993499593));
#11456=CARTESIAN_POINT('Ctrl Pts',(-1.0797140885543,0.276058653254629,9.28147192866405));
#11457=CARTESIAN_POINT('Ctrl Pts',(-1.0792869722179,-0.273490761429736,
9.30394472055128));
#11458=CARTESIAN_POINT('Ctrl Pts',(-0.816874083948392,-0.756154521252702,
9.32640385818033));
#11459=CARTESIAN_POINT('Ctrl Pts',(-0.355458797527567,-1.05362205517351,
9.34884870640624));
#11460=CARTESIAN_POINT('Ctrl Pts',(0.191577194376755,-1.09493860698716,
9.37127864639074));
#11461=CARTESIAN_POINT('Ctrl Pts',(0.571484722667441,-0.923210767165354,
9.38832293897591));
#11462=CARTESIAN_POINT('Ctrl Pts',(0.775578610165073,-0.735373724461368,
9.39999172743641));
#11463=CARTESIAN_POINT('Ctrl Pts',(0.90219668945127,-0.581077610283799,
9.40839153478326));
#11464=CARTESIAN_POINT('Ctrl Pts',(1.06423218001646,-0.268505675241936,
9.42308663622534));
#11465=CARTESIAN_POINT('Ctrl Pts',(1.08737574685665,0.14445700622961,9.43987039483926));
#11466=CARTESIAN_POINT('Ctrl Pts',(0.943512119332504,0.519555849049532,
9.45664308969273));
#11467=CARTESIAN_POINT('Ctrl Pts',(0.702595952885493,0.840663912121189,
9.47340826939813));
#11468=CARTESIAN_POINT('Ctrl Pts',(0.250731034525726,1.09066378632527,9.49435038976507));
#11469=CARTESIAN_POINT('Ctrl Pts',(-0.367646366337481,1.05577469318307,
9.51945715090945));
#11470=CARTESIAN_POINT('Ctrl Pts',(-0.872073427555176,0.697769149747224,
9.54453931621249));
#11471=CARTESIAN_POINT('Ctrl Pts',(-1.10851395153864,0.126754498956172,
9.56959609551394));
#11472=CARTESIAN_POINT('Ctrl Pts',(-1.004997965557,-0.481859237919703,9.59462670660628));
#11473=CARTESIAN_POINT('Ctrl Pts',(-0.593994937248818,-0.94163509404227,
9.61963038098806));
#11474=CARTESIAN_POINT('Ctrl Pts',(-0.0020235655980388,-1.11207375119343,
9.6446063758667));
#11475=CARTESIAN_POINT('Ctrl Pts',(0.589215999041395,-0.941636436533483,
9.66955394755264));
#11476=CARTESIAN_POINT('Ctrl Pts',(0.99867475328867,-0.483298149068583,
9.69447238340543));
#11477=CARTESIAN_POINT('Ctrl Pts',(1.10139617547556,0.121906639873499,9.71936097538517));
#11478=CARTESIAN_POINT('Ctrl Pts',(0.866669607038716,0.688301956936916,
9.74421904187644));
#11479=CARTESIAN_POINT('Ctrl Pts',(0.367204775824758,1.0425526426198,9.76904590972932));
#11480=CARTESIAN_POINT('Ctrl Pts',(-0.243395435261487,1.07672488055471,
9.79384092765142));
#11481=CARTESIAN_POINT('Ctrl Pts',(-0.777888567237211,0.781186417289152,
9.81860345995005));
#11482=CARTESIAN_POINT('Ctrl Pts',(-1.07283036518199,0.247282943918733,
9.84333289822209));
#11483=CARTESIAN_POINT('Ctrl Pts',(-1.03856704754786,-0.360866232625645,
9.86802861303319));
#11484=CARTESIAN_POINT('Ctrl Pts',(-0.686501281653619,-0.856920605922548,
9.892690097101));
#11485=CARTESIAN_POINT('Ctrl Pts',(-0.125304938207573,-1.08924443021579,
9.91731661435472));
#11486=CARTESIAN_POINT('Ctrl Pts',(0.472593334675849,-0.987703022851267,
9.94190800522239));
#11487=CARTESIAN_POINT('Ctrl Pts',(0.924078607982629,-0.583894056083662,
9.9664628819065));
#11488=CARTESIAN_POINT('Ctrl Pts',(1.03553205098759,-0.196980695813872,
9.98281022139497));
#11489=CARTESIAN_POINT('Ctrl Pts',(1.03555819462295,-0.00277911247133682,
9.99097644525911));
#11490=CARTESIAN_POINT('Origin',(1.,-2.33146835171283E-15,9.925));
#11491=CARTESIAN_POINT('Origin',(1.,-2.33146835171283E-15,9.925));
#11492=CARTESIAN_POINT('Origin',(1.,0.,7.275));
#11493=CARTESIAN_POINT('',(0.,0.,0.));
#11494=CARTESIAN_POINT('',(0.,0.,0.));
#11495=CARTESIAN_POINT('Origin',(0.,0.,0.));
#11496=CARTESIAN_POINT('',(-1.070235,-0.308121667383195,-1.31065986708547E-16));
#11497=CARTESIAN_POINT('',(-1.31065986708547E-16,-0.308121667383195,1.070235));
#11498=CARTESIAN_POINT('Origin',(0.,-0.308121667383195,0.));
#11499=CARTESIAN_POINT('Origin',(0.,-0.308121667383195,0.));
#11500=CARTESIAN_POINT('',(-1.31065986708547E-16,0.308121667383195,1.070235));
#11501=CARTESIAN_POINT('Origin',(-1.34711147906209E-16,0.,1.1));
#11502=CARTESIAN_POINT('',(-1.070235,0.308121667383195,1.31065986708547E-16));
#11503=CARTESIAN_POINT('Origin',(0.,0.308121667383195,0.));
#11504=CARTESIAN_POINT('Origin',(0.,0.308121667383195,0.));
#11505=CARTESIAN_POINT('Origin',(0.,0.,0.));
#11506=CARTESIAN_POINT('',(-1.070235,0.5,-1.31065986708547E-16));
#11507=CARTESIAN_POINT('',(-1.070235,0.,-1.31065986708547E-16));
#11508=CARTESIAN_POINT('Origin',(0.,0.5,0.));
#11509=CARTESIAN_POINT('Origin',(0.,0.,0.));
#11510=CARTESIAN_POINT('',(-0.6,-0.44,-7.34788079488412E-17));
#11511=CARTESIAN_POINT('Origin',(0.,-0.44,0.));
#11512=CARTESIAN_POINT('',(-0.6,0.44,-7.34788079488412E-17));
#11513=CARTESIAN_POINT('',(-0.6,0.,-7.34788079488412E-17));
#11514=CARTESIAN_POINT('Origin',(0.,0.44,0.));
#11515=CARTESIAN_POINT('Origin',(0.,0.47,0.));
#11516=CARTESIAN_POINT('',(-0.66,0.5,-8.08266887437253E-17));
#11517=CARTESIAN_POINT('',(-0.63,0.47,-7.71527483462832E-17));
#11518=CARTESIAN_POINT('Origin',(0.,0.5,0.));
#11519=CARTESIAN_POINT('Origin',(1.070235,0.5,0.));
#11520=CARTESIAN_POINT('Origin',(0.,0.,0.));
#11521=CARTESIAN_POINT('',(-1.070235,-0.5,-1.31065986708547E-16));
#11522=CARTESIAN_POINT('Origin',(0.,-0.5,0.));
#11523=CARTESIAN_POINT('',(-1.070235,0.,-1.31065986708547E-16));
#11524=CARTESIAN_POINT('Origin',(0.66,-0.5,0.));
#11525=CARTESIAN_POINT('',(-0.66,-0.5,-8.08266887437253E-17));
#11526=CARTESIAN_POINT('Origin',(0.,-0.5,0.));
#11527=CARTESIAN_POINT('Origin',(0.,-0.47,0.));
#11528=CARTESIAN_POINT('',(-0.63,-0.47,-7.71527483462832E-17));
#11529=CARTESIAN_POINT('',(0.,0.,0.));
#11530=CARTESIAN_POINT('Origin',(0.,0.,0.));
#11531=CARTESIAN_POINT('',(-1.129765,0.308121667383195,-1.38356309103871E-16));
#11532=CARTESIAN_POINT('',(-1.38356309103871E-16,0.308121667383195,1.129765));
#11533=CARTESIAN_POINT('Origin',(0.,0.308121667383195,0.));
#11534=CARTESIAN_POINT('Origin',(0.,0.308121667383195,0.));
#11535=CARTESIAN_POINT('',(-1.38356309103871E-16,-0.308121667383195,1.129765));
#11536=CARTESIAN_POINT('Origin',(-1.34711147906209E-16,0.,1.1));
#11537=CARTESIAN_POINT('',(-1.129765,-0.308121667383195,1.38356309103871E-16));
#11538=CARTESIAN_POINT('Origin',(0.,-0.308121667383195,0.));
#11539=CARTESIAN_POINT('Origin',(0.,-0.308121667383195,0.));
#11540=CARTESIAN_POINT('Origin',(0.,0.,0.));
#11541=CARTESIAN_POINT('',(-1.129765,-0.5,-1.38356309103871E-16));
#11542=CARTESIAN_POINT('Origin',(0.,-0.5,0.));
#11543=CARTESIAN_POINT('',(-1.129765,0.,-1.38356309103871E-16));
#11544=CARTESIAN_POINT('Origin',(1.54,0.5,0.));
#11545=CARTESIAN_POINT('',(-1.54,0.5,-1.88595607068692E-16));
#11546=CARTESIAN_POINT('Origin',(0.,0.5,0.));
#11547=CARTESIAN_POINT('',(-1.129765,0.5,-1.38356309103871E-16));
#11548=CARTESIAN_POINT('Origin',(0.,0.5,0.));
#11549=CARTESIAN_POINT('Origin',(0.,0.47,0.));
#11550=CARTESIAN_POINT('',(-1.6,0.44,-1.95943487863577E-16));
#11551=CARTESIAN_POINT('Origin',(0.,0.44,0.));
#11552=CARTESIAN_POINT('',(-1.57,0.47,-1.92269547466134E-16));
#11553=CARTESIAN_POINT('Origin',(0.,0.,0.));
#11554=CARTESIAN_POINT('',(-1.6,-0.44,-1.95943487863577E-16));
#11555=CARTESIAN_POINT('Origin',(0.,-0.44,0.));
#11556=CARTESIAN_POINT('',(-1.6,0.,-1.95943487863577E-16));
#11557=CARTESIAN_POINT('Origin',(0.,-0.47,0.));
#11558=CARTESIAN_POINT('',(-1.54,-0.5,-1.88595607068692E-16));
#11559=CARTESIAN_POINT('Origin',(0.,-0.5,0.));
#11560=CARTESIAN_POINT('',(-1.57,-0.47,-1.92269547466134E-16));
#11561=CARTESIAN_POINT('Origin',(1.129765,-0.5,0.));
#11562=CARTESIAN_POINT('Origin',(0.,0.,0.));
#11563=CARTESIAN_POINT('',(-1.129765,0.,-1.38356309103871E-16));
#11564=CARTESIAN_POINT('',(0.,0.,0.));
#11565=CARTESIAN_POINT('Origin',(1.1,0.,0.));
#11566=CARTESIAN_POINT('',(1.1,-2.23201749654651E-33,0.29765));
#11567=CARTESIAN_POINT('',(1.1,-2.23201749654651E-33,-0.29765));
#11568=CARTESIAN_POINT('Origin',(1.1,0.,0.));
#11569=CARTESIAN_POINT('Origin',(0.685838782044607,0.,-0.860014630714833));
#11570=CARTESIAN_POINT('',(0.918550922801216,-5.31350540756609E-33,-0.674432891191581));
#11571=CARTESIAN_POINT('',(0.453126641287998,8.49470414473068E-34,-1.04559637023808));
#11572=CARTESIAN_POINT('Origin',(0.685838782044607,0.,-0.860014630714833));
#11573=CARTESIAN_POINT('Origin',(-0.244773027351946,0.,-1.07242070340001));
#11574=CARTESIAN_POINT('',(0.0454142657089739,-2.23201749654651E-33,-1.1386540593921));
#11575=CARTESIAN_POINT('',(-0.534960320412865,-2.23201749654651E-33,-1.00618734740791));
#11576=CARTESIAN_POINT('Origin',(-0.244773027351946,0.,-1.07242070340001));
#11577=CARTESIAN_POINT('Origin',(-0.991065754692661,0.,-0.477272113029314));
#11578=CARTESIAN_POINT('',(-0.86192025974432,8.49470414473067E-34,-0.745445496560469));
#11579=CARTESIAN_POINT('',(-1.120211249641,-5.31350540756609E-33,-0.209098729498159));
#11580=CARTESIAN_POINT('Origin',(-0.991065754692661,0.,-0.477272113029314));
#11581=CARTESIAN_POINT('Origin',(-0.991065754692661,0.,0.477272113029314));
#11582=CARTESIAN_POINT('',(-1.120211249641,-2.23201749654651E-33,0.209098729498159));
#11583=CARTESIAN_POINT('',(-0.86192025974432,-2.23201749654651E-33,0.745445496560469));
#11584=CARTESIAN_POINT('Origin',(-0.991065754692661,0.,0.477272113029314));
#11585=CARTESIAN_POINT('Origin',(-0.244773027351946,0.,1.07242070340001));
#11586=CARTESIAN_POINT('',(-0.534960320412866,-2.23201749654651E-33,1.00618734740791));
#11587=CARTESIAN_POINT('',(0.0454142657089737,-2.23201749654651E-33,1.1386540593921));
#11588=CARTESIAN_POINT('Origin',(-0.244773027351946,0.,1.07242070340001));
#11589=CARTESIAN_POINT('Origin',(0.685838782044607,0.,0.860014630714833));
#11590=CARTESIAN_POINT('',(0.453126641287998,-2.23201749654651E-33,1.04559637023808));
#11591=CARTESIAN_POINT('',(0.918550922801216,-2.23201749654651E-33,0.674432891191581));
#11592=CARTESIAN_POINT('Origin',(0.685838782044607,0.,0.860014630714833));
#11593=CARTESIAN_POINT('',(0.,0.,0.));
#11594=CARTESIAN_POINT('Origin',(0.685838782044607,0.,0.860014630714833));
#11595=CARTESIAN_POINT('',(0.413083465285518,-0.05953,0.993751811093549));
#11596=CARTESIAN_POINT('',(0.876916659919095,-0.05953,0.623857181492959));
#11597=CARTESIAN_POINT('Ctrl Pts',(0.413083465285518,-0.05953,0.993751811093549));
#11598=CARTESIAN_POINT('Ctrl Pts',(0.419070565453383,-0.0925528133349865,
0.991263089003441));
#11599=CARTESIAN_POINT('Ctrl Pts',(0.430199341854858,-0.124911173756694,
0.986608710139579));
#11600=CARTESIAN_POINT('Ctrl Pts',(0.457978755888596,-0.177924977804098,
0.973971221090534));
#11601=CARTESIAN_POINT('Ctrl Pts',(0.473077587363685,-0.199697230012983,
0.966820759530997));
#11602=CARTESIAN_POINT('Ctrl Pts',(0.507057380724533,-0.237895043532788,
0.949440676105255));
#11603=CARTESIAN_POINT('Ctrl Pts',(0.525933334162555,-0.254319232363049,
0.939198248544428));
#11604=CARTESIAN_POINT('Ctrl Pts',(0.564362943424238,-0.28018331644634,
0.916597376014514));
#11605=CARTESIAN_POINT('Ctrl Pts',(0.585840553788742,-0.29104845371857,
0.903141581680914));
#11606=CARTESIAN_POINT('Ctrl Pts',(0.629305439856167,-0.30527573347708,
0.873412008702649));
#11607=CARTESIAN_POINT('Ctrl Pts',(0.651278921914856,-0.308638795020976,
0.857118508332695));
#11608=CARTESIAN_POINT('Ctrl Pts',(0.690705563850638,-0.308638795020976,
0.825676810575914));
#11609=CARTESIAN_POINT('Ctrl Pts',(0.711480111898423,-0.30527573347708,
0.807879894508811));
#11610=CARTESIAN_POINT('Ctrl Pts',(0.750136149454208,-0.29104845371857,
0.772120216227122));
#11611=CARTESIAN_POINT('Ctrl Pts',(0.768033796848072,-0.28018331644634,
0.754175290318038));
#11612=CARTESIAN_POINT('Ctrl Pts',(0.798619410861634,-0.254319232363049,
0.721738358858166));
#11613=CARTESIAN_POINT('Ctrl Pts',(0.812805334167529,-0.237895043532788,
0.705614819529209));
#11614=CARTESIAN_POINT('Ctrl Pts',(0.837310877969633,-0.199697230012983,
0.676354402927683));
#11615=CARTESIAN_POINT('Ctrl Pts',(0.847641868610495,-0.177924977804098,
0.663225258065736));
#11616=CARTESIAN_POINT('Ctrl Pts',(0.866144010579847,-0.124911173756694,
0.638954437806245));
#11617=CARTESIAN_POINT('Ctrl Pts',(0.873158080166742,-0.0925528133349865,
0.62914037979579));
#11618=CARTESIAN_POINT('Ctrl Pts',(0.876916659919095,-0.05953,0.623857181492959));
#11619=CARTESIAN_POINT('',(0.437601487681057,-0.05953,1.03511272300331));
#11620=CARTESIAN_POINT('Origin',(0.685838782044607,-0.05953,0.860014630714833));
#11621=CARTESIAN_POINT('',(0.911784794170997,-0.05953,0.656964154625313));
#11622=CARTESIAN_POINT('Ctrl Pts',(0.911784794170998,-0.0595300000000001,
0.656964154625312));
#11623=CARTESIAN_POINT('Ctrl Pts',(0.909827729890942,-0.0762225747374255,
0.659680317203144));
#11624=CARTESIAN_POINT('Ctrl Pts',(0.907004864562642,-0.0928409665394228,
0.663576540841106));
#11625=CARTESIAN_POINT('Ctrl Pts',(0.895234408667242,-0.144299303100741,
0.679480524217551));
#11626=CARTESIAN_POINT('Ctrl Pts',(0.882797231409153,-0.177024326825049,
0.695831250979106));
#11627=CARTESIAN_POINT('Ctrl Pts',(0.854332839576145,-0.227269801620064,
0.73042219438957));
#11628=CARTESIAN_POINT('Ctrl Pts',(0.834863020612702,-0.251265615809407,
0.752807465209441));
#11629=CARTESIAN_POINT('Ctrl Pts',(0.800439809856111,-0.279889827963178,
0.789147407129766));
#11630=CARTESIAN_POINT('Ctrl Pts',(0.781998747691871,-0.290879136862659,
0.80756613568454));
#11631=CARTESIAN_POINT('Ctrl Pts',(0.742239891936898,-0.305251990234487,
0.844254137480382));
#11632=CARTESIAN_POINT('Ctrl Pts',(0.720906778729541,-0.308638795020976,
0.862505527716294));
#11633=CARTESIAN_POINT('Ctrl Pts',(0.680463863683392,-0.308638795020976,
0.894757676234429));
#11634=CARTESIAN_POINT('Ctrl Pts',(0.657923009631182,-0.305251990234488,
0.91149460735272));
#11635=CARTESIAN_POINT('Ctrl Pts',(0.613307674922609,-0.290879136862659,
0.942092777160053));
#11636=CARTESIAN_POINT('Ctrl Pts',(0.591247219971725,-0.279889827963178,
0.955972930713954));
#11637=CARTESIAN_POINT('Ctrl Pts',(0.548158511259202,-0.251265615809407,
0.981446681891443));
#11638=CARTESIAN_POINT('Ctrl Pts',(0.522002043615455,-0.227269801620063,
0.995447160474328));
#11639=CARTESIAN_POINT('Ctrl Pts',(0.481944444320713,-0.177024326825049,
1.01550068154148));
#11640=CARTESIAN_POINT('Ctrl Pts',(0.463236132117164,-0.14429930310074,
1.0239876538093));
#11641=CARTESIAN_POINT('Ctrl Pts',(0.445111721969657,-0.0928409665394226,
1.03192403056628));
#11642=CARTESIAN_POINT('Ctrl Pts',(0.440685038163619,-0.0762225747374254,
1.03380912944435));
#11643=CARTESIAN_POINT('Ctrl Pts',(0.437601487681056,-0.05953,1.03511272300331));
#11644=CARTESIAN_POINT('Origin',(0.685838782044607,-0.05953,0.860014630714833));
#11645=CARTESIAN_POINT('Origin',(0.,-0.208355,0.));
#11646=CARTESIAN_POINT('',(0.0548532617164168,-0.05953,1.12247250791415));
#11647=CARTESIAN_POINT('Origin',(0.,-0.05953,0.));
#11648=CARTESIAN_POINT('',(-0.536443649899848,-0.05953,0.987512846410683));
#11649=CARTESIAN_POINT('Ctrl Pts',(0.0548532617164173,-0.0595300000000001,
1.12247250791414));
#11650=CARTESIAN_POINT('Ctrl Pts',(0.05150947068137,-0.0762225747374254,
1.12263591311425));
#11651=CARTESIAN_POINT('Ctrl Pts',(0.0467032526342597,-0.0928409665394227,
1.12285816383385));
#11652=CARTESIAN_POINT('Ctrl Pts',(0.0269302585198975,-0.144299303100741,
1.12357162229597));
#11653=CARTESIAN_POINT('Ctrl Pts',(0.006392292392153,-0.177024326825049,
1.12404235695137));
#11654=CARTESIAN_POINT('Ctrl Pts',(-0.0383992541984087,-0.227269801620063,
1.12335509974011));
#11655=CARTESIAN_POINT('Ctrl Pts',(-0.0680399972366993,-0.251265615809407,
1.12208997038458));
#11656=CARTESIAN_POINT('Ctrl Pts',(-0.117914228755037,-0.279889827963178,
1.1178344036749));
#11657=CARTESIAN_POINT('Ctrl Pts',(-0.14381238480104,-0.290879136862659,
1.11490049012186));
#11658=CARTESIAN_POINT('Ctrl Pts',(-0.19728546073067,-0.305251990234488,
1.10669035995599));
#11659=CARTESIAN_POINT('Ctrl Pts',(-0.224855950742601,-0.308638795020976,
1.10139101611326));
#11660=CARTESIAN_POINT('Ctrl Pts',(-0.275287440920027,-0.308638795020976,
1.0898803575765));
#11661=CARTESIAN_POINT('Ctrl Pts',(-0.302426893214945,-0.305251990234488,
1.08269251410343));
#11662=CARTESIAN_POINT('Ctrl Pts',(-0.35416671187353,-0.290879136862659,
1.06688848765783));
#11663=CARTESIAN_POINT('Ctrl Pts',(-0.3787731215897,-0.279889827963178,
1.05829506364875));
#11664=CARTESIAN_POINT('Ctrl Pts',(-0.425554672694338,-0.251265615809407,
1.04048957871266));
#11665=CARTESIAN_POINT('Ctrl Pts',(-0.452808978448581,-0.227269801620063,
1.02876878445619));
#11666=CARTESIAN_POINT('Ctrl Pts',(-0.493462957200432,-0.177024326825049,
1.0099536580922));
#11667=CARTESIAN_POINT('Ctrl Pts',(-0.511762781179148,-0.14429930310074,
1.00061845128527));
#11668=CARTESIAN_POINT('Ctrl Pts',(-0.529268075276157,-0.0928409665394226,
0.991396466802468));
#11669=CARTESIAN_POINT('Ctrl Pts',(-0.533501897135713,-0.0762225747374254,
0.989110885965947));
#11670=CARTESIAN_POINT('Ctrl Pts',(-0.536443649899848,-0.0595300000000001,
0.987512846410683));
#11671=CARTESIAN_POINT('',(-0.843383895613249,-0.05953,0.742736168477219));
#11672=CARTESIAN_POINT('Origin',(0.,-0.05953,0.));
#11673=CARTESIAN_POINT('',(-1.10653577764992,-0.05953,0.196295654879792));
#11674=CARTESIAN_POINT('Ctrl Pts',(-0.843383895613249,-0.0595300000000001,
0.742736168477219));
#11675=CARTESIAN_POINT('Ctrl Pts',(-0.84559647055299,-0.0762225747374255,
0.740223768851062));
#11676=CARTESIAN_POINT('Ctrl Pts',(-0.848766861100456,-0.0928409665394227,
0.736604687327351));
#11677=CARTESIAN_POINT('Ctrl Pts',(-0.861652925570091,-0.144299303100741,
0.721590372101268));
#11678=CARTESIAN_POINT('Ctrl Pts',(-0.87482617317514,-0.177024326825049,
0.705826641853758));
#11679=CARTESIAN_POINT('Ctrl Pts',(-0.902215926359523,-0.227269801620063,
0.670378702718353));
#11680=CARTESIAN_POINT('Ctrl Pts',(-0.919707509403859,-0.251265615809407,
0.646415841396062));
#11681=CARTESIAN_POINT('Ctrl Pts',(-0.947476448101718,-0.279889827963178,
0.604769294586516));
#11682=CARTESIAN_POINT('Ctrl Pts',(-0.961329858300736,-0.290879136862659,
0.582692035672022));
#11683=CARTESIAN_POINT('Ctrl Pts',(-0.988250837578047,-0.305251990234488,
0.535766169015486));
#11684=CARTESIAN_POINT('Ctrl Pts',(-1.00129756308006,-0.308638795020976,
0.510906605094603));
#11685=CARTESIAN_POINT('Ctrl Pts',(-1.02374168767024,-0.308638795020976,
0.46430090015576));
#11686=CARTESIAN_POINT('Ctrl Pts',(-1.03504317708586,-0.305251990234488,
0.438600874831839));
#11687=CARTESIAN_POINT('Ctrl Pts',(-1.05494634094458,-0.290879136862659,
0.388295406390235));
#11688=CARTESIAN_POINT('Ctrl Pts',(-1.06356957703048,-0.279889827963178,
0.363699428370917));
#11689=CARTESIAN_POINT('Ctrl Pts',(-1.0788165083757,-0.251265615809407,
0.316022600643821));
#11690=CARTESIAN_POINT('Ctrl Pts',(-1.08664560412098,-0.227269801620063,
0.287406530683752));
#11691=CARTESIAN_POINT('Ctrl Pts',(-1.09728268713976,-0.177024326825049,
0.243890930799337));
#11692=CARTESIAN_POINT('Ctrl Pts',(-1.10139388218929,-0.144299303100741,
0.22376314604679));
#11693=CARTESIAN_POINT('Ctrl Pts',(-1.10509821673782,-0.0928409665394227,
0.204327142733961));
#11694=CARTESIAN_POINT('Ctrl Pts',(-1.10595102243643,-0.0762225747374254,
0.199591971170104));
#11695=CARTESIAN_POINT('Ctrl Pts',(-1.10653577764992,-0.0595300000000001,
0.196295654879792));
#11696=CARTESIAN_POINT('',(-1.123812,-0.05953,1.37627276864339E-16));
#11697=CARTESIAN_POINT('Origin',(0.,-0.05953,0.));
#11698=CARTESIAN_POINT('',(-1.123812,-0.35718,1.37627276864339E-16));
#11699=CARTESIAN_POINT('',(-1.123812,-0.208355,1.37627276864339E-16));
#11700=CARTESIAN_POINT('Origin',(0.,-0.35718,0.));
#11701=CARTESIAN_POINT('',(-1.10653577764992,-0.05953,-0.196295654879793));
#11702=CARTESIAN_POINT('Origin',(0.,-0.05953,0.));
#11703=CARTESIAN_POINT('',(-0.843383895613249,-0.05953,-0.742736168477219));
#11704=CARTESIAN_POINT('Ctrl Pts',(-1.10653577764992,-0.0595300000000001,
-0.196295654879792));
#11705=CARTESIAN_POINT('Ctrl Pts',(-1.10595102243643,-0.0762225747374255,
-0.199591971170104));
#11706=CARTESIAN_POINT('Ctrl Pts',(-1.10509821673782,-0.0928409665394228,
-0.204327142733962));
#11707=CARTESIAN_POINT('Ctrl Pts',(-1.10139388218929,-0.144299303100741,
-0.22376314604679));
#11708=CARTESIAN_POINT('Ctrl Pts',(-1.09728268713976,-0.177024326825049,
-0.243890930799338));
#11709=CARTESIAN_POINT('Ctrl Pts',(-1.08664560412098,-0.227269801620063,
-0.287406530683753));
#11710=CARTESIAN_POINT('Ctrl Pts',(-1.0788165083757,-0.251265615809407,
-0.316022600643821));
#11711=CARTESIAN_POINT('Ctrl Pts',(-1.06356957703048,-0.279889827963178,
-0.363699428370918));
#11712=CARTESIAN_POINT('Ctrl Pts',(-1.05494634094458,-0.290879136862659,
-0.388295406390235));
#11713=CARTESIAN_POINT('Ctrl Pts',(-1.03504317708586,-0.305251990234488,
-0.438600874831839));
#11714=CARTESIAN_POINT('Ctrl Pts',(-1.02374168767024,-0.308638795020976,
-0.46430090015576));
#11715=CARTESIAN_POINT('Ctrl Pts',(-1.00129756308006,-0.308638795020976,
-0.510906605094603));
#11716=CARTESIAN_POINT('Ctrl Pts',(-0.988250837578047,-0.305251990234488,
-0.535766169015486));
#11717=CARTESIAN_POINT('Ctrl Pts',(-0.961329858300736,-0.290879136862659,
-0.582692035672022));
#11718=CARTESIAN_POINT('Ctrl Pts',(-0.947476448101718,-0.279889827963178,
-0.604769294586516));
#11719=CARTESIAN_POINT('Ctrl Pts',(-0.919707509403859,-0.251265615809407,
-0.646415841396062));
#11720=CARTESIAN_POINT('Ctrl Pts',(-0.902215926359523,-0.227269801620064,
-0.670378702718353));
#11721=CARTESIAN_POINT('Ctrl Pts',(-0.87482617317514,-0.177024326825049,
-0.705826641853758));
#11722=CARTESIAN_POINT('Ctrl Pts',(-0.861652925570091,-0.144299303100741,
-0.721590372101268));
#11723=CARTESIAN_POINT('Ctrl Pts',(-0.848766861100456,-0.0928409665394229,
-0.736604687327351));
#11724=CARTESIAN_POINT('Ctrl Pts',(-0.84559647055299,-0.0762225747374255,
-0.740223768851063));
#11725=CARTESIAN_POINT('Ctrl Pts',(-0.843383895613249,-0.0595300000000001,
-0.742736168477219));
#11726=CARTESIAN_POINT('',(-0.536443649899847,-0.05953,-0.987512846410683));
#11727=CARTESIAN_POINT('Origin',(0.,-0.05953,0.));
#11728=CARTESIAN_POINT('',(0.0548532617164172,-0.05953,-1.12247250791415));
#11729=CARTESIAN_POINT('Ctrl Pts',(-0.536443649899848,-0.0595300000000001,
-0.987512846410683));
#11730=CARTESIAN_POINT('Ctrl Pts',(-0.533501897135712,-0.0762225747374254,
-0.989110885965947));
#11731=CARTESIAN_POINT('Ctrl Pts',(-0.529268075276156,-0.0928409665394227,
-0.991396466802469));
#11732=CARTESIAN_POINT('Ctrl Pts',(-0.511762781179147,-0.144299303100741,
-1.00061845128527));
#11733=CARTESIAN_POINT('Ctrl Pts',(-0.493462957200432,-0.177024326825049,
-1.0099536580922));
#11734=CARTESIAN_POINT('Ctrl Pts',(-0.45280897844858,-0.227269801620063,
-1.02876878445619));
#11735=CARTESIAN_POINT('Ctrl Pts',(-0.425554672694337,-0.251265615809407,
-1.04048957871266));
#11736=CARTESIAN_POINT('Ctrl Pts',(-0.3787731215897,-0.279889827963178,
-1.05829506364875));
#11737=CARTESIAN_POINT('Ctrl Pts',(-0.354166711873529,-0.290879136862659,
-1.06688848765783));
#11738=CARTESIAN_POINT('Ctrl Pts',(-0.302426893214944,-0.305251990234488,
-1.08269251410343));
#11739=CARTESIAN_POINT('Ctrl Pts',(-0.275287440920027,-0.308638795020976,
-1.0898803575765));
#11740=CARTESIAN_POINT('Ctrl Pts',(-0.224855950742601,-0.308638795020976,
-1.10139101611326));
#11741=CARTESIAN_POINT('Ctrl Pts',(-0.19728546073067,-0.305251990234488,
-1.10669035995599));
#11742=CARTESIAN_POINT('Ctrl Pts',(-0.143812384801039,-0.290879136862659,
-1.11490049012186));
#11743=CARTESIAN_POINT('Ctrl Pts',(-0.117914228755037,-0.279889827963178,
-1.1178344036749));
#11744=CARTESIAN_POINT('Ctrl Pts',(-0.0680399972366989,-0.251265615809407,
-1.12208997038458));
#11745=CARTESIAN_POINT('Ctrl Pts',(-0.0383992541984084,-0.227269801620063,
-1.12335509974011));
#11746=CARTESIAN_POINT('Ctrl Pts',(0.00639229239215326,-0.177024326825049,
-1.12404235695137));
#11747=CARTESIAN_POINT('Ctrl Pts',(0.0269302585198977,-0.144299303100741,
-1.12357162229597));
#11748=CARTESIAN_POINT('Ctrl Pts',(0.04670325263426,-0.0928409665394228,
-1.12285816383385));
#11749=CARTESIAN_POINT('Ctrl Pts',(0.0515094706813703,-0.0762225747374255,
-1.12263591311425));
#11750=CARTESIAN_POINT('Ctrl Pts',(0.0548532617164176,-0.0595300000000001,
-1.12247250791414));
#11751=CARTESIAN_POINT('',(0.437601487681057,-0.05953,-1.03511272300331));
#11752=CARTESIAN_POINT('Origin',(0.,-0.05953,0.));
#11753=CARTESIAN_POINT('',(0.911784794170997,-0.05953,-0.656964154625313));
#11754=CARTESIAN_POINT('Ctrl Pts',(0.437601487681056,-0.0595300000000001,
-1.03511272300331));
#11755=CARTESIAN_POINT('Ctrl Pts',(0.440685038163619,-0.0762225747374255,
-1.03380912944435));
#11756=CARTESIAN_POINT('Ctrl Pts',(0.445111721969657,-0.0928409665394228,
-1.03192403056628));
#11757=CARTESIAN_POINT('Ctrl Pts',(0.463236132117164,-0.144299303100741,
-1.0239876538093));
#11758=CARTESIAN_POINT('Ctrl Pts',(0.481944444320713,-0.177024326825049,
-1.01550068154148));
#11759=CARTESIAN_POINT('Ctrl Pts',(0.522002043615455,-0.227269801620064,
-0.995447160474328));
#11760=CARTESIAN_POINT('Ctrl Pts',(0.548158511259203,-0.251265615809407,
-0.981446681891443));
#11761=CARTESIAN_POINT('Ctrl Pts',(0.591247219971725,-0.279889827963178,
-0.955972930713954));
#11762=CARTESIAN_POINT('Ctrl Pts',(0.613307674922609,-0.290879136862659,
-0.942092777160053));
#11763=CARTESIAN_POINT('Ctrl Pts',(0.657923009631182,-0.305251990234487,
-0.91149460735272));
#11764=CARTESIAN_POINT('Ctrl Pts',(0.680463863683393,-0.308638795020976,
-0.894757676234429));
#11765=CARTESIAN_POINT('Ctrl Pts',(0.720906778729542,-0.308638795020976,
-0.862505527716294));
#11766=CARTESIAN_POINT('Ctrl Pts',(0.742239891936899,-0.305251990234488,
-0.844254137480381));
#11767=CARTESIAN_POINT('Ctrl Pts',(0.781998747691872,-0.290879136862659,
-0.80756613568454));
#11768=CARTESIAN_POINT('Ctrl Pts',(0.800439809856112,-0.279889827963178,
-0.789147407129765));
#11769=CARTESIAN_POINT('Ctrl Pts',(0.834863020612702,-0.251265615809407,
-0.752807465209441));
#11770=CARTESIAN_POINT('Ctrl Pts',(0.854332839576145,-0.227269801620064,
-0.73042219438957));
#11771=CARTESIAN_POINT('Ctrl Pts',(0.882797231409153,-0.177024326825049,
-0.695831250979106));
#11772=CARTESIAN_POINT('Ctrl Pts',(0.895234408667242,-0.144299303100741,
-0.679480524217551));
#11773=CARTESIAN_POINT('Ctrl Pts',(0.907004864562642,-0.0928409665394228,
-0.663576540841106));
#11774=CARTESIAN_POINT('Ctrl Pts',(0.909827729890942,-0.0762225747374256,
-0.659680317203144));
#11775=CARTESIAN_POINT('Ctrl Pts',(0.911784794170998,-0.0595300000000001,
-0.656964154625312));
#11776=CARTESIAN_POINT('',(1.08212377959455,-0.05953,-0.303251606722892));
#11777=CARTESIAN_POINT('Origin',(0.,-0.05953,0.));
#11778=CARTESIAN_POINT('',(1.08212377959455,-0.05953,0.303251606722892));
#11779=CARTESIAN_POINT('Ctrl Pts',(1.08212377959455,-0.0595300000000001,
-0.303251606722892));
#11780=CARTESIAN_POINT('Ctrl Pts',(1.0830271513892,-0.0762225747374255,
-0.300028012588062));
#11781=CARTESIAN_POINT('Ctrl Pts',(1.08431331394788,-0.0928409665394228,
-0.2953917518996));
#11782=CARTESIAN_POINT('Ctrl Pts',(1.08940878963422,-0.144299303100741,
-0.276273267473431));
#11783=CARTESIAN_POINT('Ctrl Pts',(1.09443784939331,-0.177024326825049,
-0.256354979351213));
#11784=CARTESIAN_POINT('Ctrl Pts',(1.10373487993589,-0.227269801620064,
-0.212533521233765));
#11785=CARTESIAN_POINT('Ctrl Pts',(1.10909715583869,-0.251265615809407,
-0.183354415742157));
#11786=CARTESIAN_POINT('Ctrl Pts',(1.1160463456491,-0.279889827963178,-0.133783682657561));
#11787=CARTESIAN_POINT('Ctrl Pts',(1.11894887330541,-0.290879136862659,
-0.107881990270302));
#11788=CARTESIAN_POINT('Ctrl Pts',(1.12284346704144,-0.305251990234488,
-0.0539226701638766));
#11789=CARTESIAN_POINT('Ctrl Pts',(1.123812,-0.308638795020976,-0.025864214957475));
#11790=CARTESIAN_POINT('Ctrl Pts',(1.123812,-0.308638795020976,0.025864214957475));
#11791=CARTESIAN_POINT('Ctrl Pts',(1.12284346704144,-0.305251990234488,
0.0539226701638766));
#11792=CARTESIAN_POINT('Ctrl Pts',(1.11894887330541,-0.290879136862659,
0.107881990270302));
#11793=CARTESIAN_POINT('Ctrl Pts',(1.1160463456491,-0.279889827963178,0.133783682657561));
#11794=CARTESIAN_POINT('Ctrl Pts',(1.10909715583869,-0.251265615809407,
0.183354415742157));
#11795=CARTESIAN_POINT('Ctrl Pts',(1.10373487993589,-0.227269801620064,
0.212533521233765));
#11796=CARTESIAN_POINT('Ctrl Pts',(1.09443784939331,-0.177024326825049,
0.256354979351213));
#11797=CARTESIAN_POINT('Ctrl Pts',(1.08940878963422,-0.144299303100741,
0.276273267473431));
#11798=CARTESIAN_POINT('Ctrl Pts',(1.08431331394788,-0.0928409665394228,
0.2953917518996));
#11799=CARTESIAN_POINT('Ctrl Pts',(1.0830271513892,-0.0762225747374255,
0.300028012588062));
#11800=CARTESIAN_POINT('Ctrl Pts',(1.08212377959455,-0.0595300000000001,
0.303251606722892));
#11801=CARTESIAN_POINT('Origin',(0.,-0.05953,0.));
#11802=CARTESIAN_POINT('Origin',(0.,-0.05953,0.));
#11803=CARTESIAN_POINT('',(0.0589974094846122,-0.05953,1.07456964270265));
#11804=CARTESIAN_POINT('Origin',(0.,-0.05953,0.));
#11805=CARTESIAN_POINT('Origin',(-0.244773027351946,-0.05953,1.07242070340001));
#11806=CARTESIAN_POINT('Origin',(-0.244773027351946,0.,1.07242070340001));
#11807=CARTESIAN_POINT('',(-0.519393123750572,-0.05953,0.942555777842682));
#11808=CARTESIAN_POINT('Ctrl Pts',(-0.519393123750572,-0.05953,0.942555777842682));
#11809=CARTESIAN_POINT('Ctrl Pts',(-0.513714466572041,-0.0925528133349865,
0.945684988399766));
#11810=CARTESIAN_POINT('Ctrl Pts',(-0.503136848051455,-0.124911173756694,
0.951483858396181));
#11811=CARTESIAN_POINT('Ctrl Pts',(-0.47593627990192,-0.177924977804098,
0.965323333309091));
#11812=CARTESIAN_POINT('Ctrl Pts',(-0.460931856495794,-0.199697230012983,
0.972669835243841));
#11813=CARTESIAN_POINT('Ctrl Pts',(-0.426157505475872,-0.237895043532788,
0.988400002689705));
#11814=CARTESIAN_POINT('Ctrl Pts',(-0.406380688682952,-0.254319232363049,
0.996771768218699));
#11815=CARTESIAN_POINT('Ctrl Pts',(-0.364750145543744,-0.28018331644634,
1.01272583306292));
#11816=CARTESIAN_POINT('Ctrl Pts',(-0.340838910881557,-0.29104845371857,
1.02112815447116));
#11817=CARTESIAN_POINT('Ctrl Pts',(-0.290495481564827,-0.30527573347708,
1.036574285215));
#11818=CARTESIAN_POINT('Ctrl Pts',(-0.264056468041074,-0.308638795020976,
1.04359501395068));
#11819=CARTESIAN_POINT('Ctrl Pts',(-0.214892249704082,-0.308638795020976,
1.05481642595959));
#11820=CARTESIAN_POINT('Ctrl Pts',(-0.188025341585962,-0.30527573347708,
1.05996242598502));
#11821=CARTESIAN_POINT('Ctrl Pts',(-0.135965654106109,-0.29104845371857,
1.06788913840721));
#11822=CARTESIAN_POINT('Ctrl Pts',(-0.110776745452494,-0.28018331644634,
1.07069360430242));
#11823=CARTESIAN_POINT('Ctrl Pts',(-0.0663467128214646,-0.254319232363049,
1.07438230428002));
#11824=CARTESIAN_POINT('Ctrl Pts',(-0.0448960436540983,-0.237895043532788,
1.07542044338697));
#11825=CARTESIAN_POINT('Ctrl Pts',(-0.00674037211528124,-0.199697230012983,
1.07633607767727));
#11826=CARTESIAN_POINT('Ctrl Pts',(0.00996567398334777,-0.177924977804098,
1.07622728347683));
#11827=CARTESIAN_POINT('Ctrl Pts',(0.0404772621979741,-0.124911173756694,
1.07556023164702));
#11828=CARTESIAN_POINT('Ctrl Pts',(0.0525234025782719,-0.0925528133349865,
1.07492508698591));
#11829=CARTESIAN_POINT('Ctrl Pts',(0.0589974094846124,-0.05953,1.07456964270265));
#11830=CARTESIAN_POINT('Origin',(-0.244773027351946,-0.05953,1.07242070340001));
#11831=CARTESIAN_POINT('Origin',(0.,-0.05953,0.));
#11832=CARTESIAN_POINT('',(-0.803348093619616,-0.05953,0.716109245731214));
#11833=CARTESIAN_POINT('Origin',(0.,-0.05953,0.));
#11834=CARTESIAN_POINT('Origin',(-0.991065754692661,-0.05953,0.477272113029314));
#11835=CARTESIAN_POINT('Origin',(-0.991065754692661,0.,0.477272113029314));
#11836=CARTESIAN_POINT('',(-1.06075609691358,-0.05953,0.181596019242328));
#11837=CARTESIAN_POINT('Ctrl Pts',(-1.06075609691358,-0.05953,0.181596019242328));
#11838=CARTESIAN_POINT('Ctrl Pts',(-1.05966202740332,-0.0925528133349865,
0.187986803072856));
#11839=CARTESIAN_POINT('Ctrl Pts',(-1.05760072925372,-0.124911173756694,
0.199872254546857));
#11840=CARTESIAN_POINT('Ctrl Pts',(-1.05146158959546,-0.177924977804098,
0.22976728653846));
#11841=CARTESIAN_POINT('Ctrl Pts',(-1.04785021111757,-0.199697230012983,
0.246078686169301));
#11842=CARTESIAN_POINT('Ctrl Pts',(-1.03846709802406,-0.237895043532788,
0.283073967563097));
#11843=CARTESIAN_POINT('Ctrl Pts',(-1.03268176429485,-0.254319232363049,
0.303755815985685));
#11844=CARTESIAN_POINT('Ctrl Pts',(-1.01919893537026,-0.28018331644634,
0.346251081972725));
#11845=CARTESIAN_POINT('Ctrl Pts',(-1.01085972381132,-0.29104845371857,
0.370184399726282));
#11846=CARTESIAN_POINT('Ctrl Pts',(-0.99154738033959,-0.30527573347708,
0.419174982698463));
#11847=CARTESIAN_POINT('Ctrl Pts',(-0.980551951791748,-0.308638795020976,
0.444223188605045));
#11848=CARTESIAN_POINT('Ctrl Pts',(-0.958671816228589,-0.308638795020976,
0.489657758261848));
#11849=CARTESIAN_POINT('Ctrl Pts',(-0.945943877838127,-0.30527573347708,
0.51387163140139));
#11850=CARTESIAN_POINT('Ctrl Pts',(-0.91968254693063,-0.29104845371857,
0.559515758398093));
#11851=CARTESIAN_POINT('Ctrl Pts',(-0.906170138993533,-0.28018331644634,
0.580957796077825));
#11852=CARTESIAN_POINT('Ctrl Pts',(-0.8813524085237,-0.254319232363049,
0.617994461173994));
#11853=CARTESIAN_POINT('Ctrl Pts',(-0.868789784891799,-0.237895043532788,
0.635412538795143));
#11854=CARTESIAN_POINT('Ctrl Pts',(-0.845715984518854,-0.199697230012983,
0.66581473268113));
#11855=CARTESIAN_POINT('Ctrl Pts',(-0.835214876415962,-0.177924977804098,
0.678808213394124));
#11856=CARTESIAN_POINT('Ctrl Pts',(-0.815669690204649,-0.124911173756694,
0.702247233627224));
#11857=CARTESIAN_POINT('Ctrl Pts',(-0.807662468433796,-0.0925528133349865,
0.711269279199861));
#11858=CARTESIAN_POINT('Ctrl Pts',(-0.803348093619616,-0.05953,0.716109245731214));
#11859=CARTESIAN_POINT('Origin',(-0.991065754692661,-0.05953,0.477272113029314));
#11860=CARTESIAN_POINT('Origin',(0.,-0.05953,0.));
#11861=CARTESIAN_POINT('',(-1.076188,-0.05953,1.31795018948079E-16));
#11862=CARTESIAN_POINT('Origin',(0.,-0.05953,0.));
#11863=CARTESIAN_POINT('',(-1.06075609691358,-0.05953,-0.181596019242328));
#11864=CARTESIAN_POINT('Origin',(0.,-0.05953,0.));
#11865=CARTESIAN_POINT('Origin',(-0.991065754692661,-0.05953,-0.477272113029314));
#11866=CARTESIAN_POINT('Origin',(-0.991065754692661,0.,-0.477272113029314));
#11867=CARTESIAN_POINT('',(-0.803348093619616,-0.05953,-0.716109245731215));
#11868=CARTESIAN_POINT('Ctrl Pts',(-0.803348093619616,-0.05953,-0.716109245731215));
#11869=CARTESIAN_POINT('Ctrl Pts',(-0.807662468433795,-0.0925528133349865,
-0.711269279199862));
#11870=CARTESIAN_POINT('Ctrl Pts',(-0.815669690204649,-0.124911173756694,
-0.702247233627224));
#11871=CARTESIAN_POINT('Ctrl Pts',(-0.835214876415962,-0.177924977804098,
-0.678808213394124));
#11872=CARTESIAN_POINT('Ctrl Pts',(-0.845715984518854,-0.199697230012983,
-0.66581473268113));
#11873=CARTESIAN_POINT('Ctrl Pts',(-0.868789784891799,-0.237895043532788,
-0.635412538795143));
#11874=CARTESIAN_POINT('Ctrl Pts',(-0.8813524085237,-0.254319232363049,
-0.617994461173994));
#11875=CARTESIAN_POINT('Ctrl Pts',(-0.906170138993533,-0.28018331644634,
-0.580957796077826));
#11876=CARTESIAN_POINT('Ctrl Pts',(-0.91968254693063,-0.29104845371857,
-0.559515758398093));
#11877=CARTESIAN_POINT('Ctrl Pts',(-0.945943877838127,-0.30527573347708,
-0.51387163140139));
#11878=CARTESIAN_POINT('Ctrl Pts',(-0.958671816228589,-0.308638795020976,
-0.489657758261848));
#11879=CARTESIAN_POINT('Ctrl Pts',(-0.980551951791748,-0.308638795020976,
-0.444223188605045));
#11880=CARTESIAN_POINT('Ctrl Pts',(-0.99154738033959,-0.30527573347708,
-0.419174982698463));
#11881=CARTESIAN_POINT('Ctrl Pts',(-1.01085972381132,-0.29104845371857,
-0.370184399726282));
#11882=CARTESIAN_POINT('Ctrl Pts',(-1.01919893537026,-0.28018331644634,
-0.346251081972725));
#11883=CARTESIAN_POINT('Ctrl Pts',(-1.03268176429485,-0.254319232363049,
-0.303755815985685));
#11884=CARTESIAN_POINT('Ctrl Pts',(-1.03846709802406,-0.237895043532788,
-0.283073967563097));
#11885=CARTESIAN_POINT('Ctrl Pts',(-1.04785021111757,-0.199697230012983,
-0.246078686169302));
#11886=CARTESIAN_POINT('Ctrl Pts',(-1.05146158959546,-0.177924977804098,
-0.229767286538461));
#11887=CARTESIAN_POINT('Ctrl Pts',(-1.05760072925372,-0.124911173756694,
-0.199872254546858));
#11888=CARTESIAN_POINT('Ctrl Pts',(-1.05966202740332,-0.0925528133349864,
-0.187986803072857));
#11889=CARTESIAN_POINT('Ctrl Pts',(-1.06075609691358,-0.05953,-0.181596019242328));
#11890=CARTESIAN_POINT('Origin',(-0.991065754692661,-0.05953,-0.477272113029314));
#11891=CARTESIAN_POINT('Origin',(0.,-0.05953,0.));
#11892=CARTESIAN_POINT('',(-0.519393123750572,-0.05953,-0.942555777842682));
#11893=CARTESIAN_POINT('Origin',(0.,-0.05953,0.));
#11894=CARTESIAN_POINT('Origin',(-0.244773027351946,-0.05953,-1.07242070340001));
#11895=CARTESIAN_POINT('Origin',(-0.244773027351946,0.,-1.07242070340001));
#11896=CARTESIAN_POINT('',(0.0589974094846125,-0.05953,-1.07456964270265));
#11897=CARTESIAN_POINT('Ctrl Pts',(0.0589974094846127,-0.05953,-1.07456964270265));
#11898=CARTESIAN_POINT('Ctrl Pts',(0.0525234025782722,-0.0925528133349865,
-1.07492508698591));
#11899=CARTESIAN_POINT('Ctrl Pts',(0.0404772621979744,-0.124911173756694,
-1.07556023164702));
#11900=CARTESIAN_POINT('Ctrl Pts',(0.0099656739833481,-0.177924977804098,
-1.07622728347683));
#11901=CARTESIAN_POINT('Ctrl Pts',(-0.00674037211528096,-0.199697230012983,
-1.07633607767727));
#11902=CARTESIAN_POINT('Ctrl Pts',(-0.044896043654098,-0.237895043532788,
-1.07542044338697));
#11903=CARTESIAN_POINT('Ctrl Pts',(-0.0663467128214644,-0.254319232363049,
-1.07438230428002));
#11904=CARTESIAN_POINT('Ctrl Pts',(-0.110776745452493,-0.28018331644634,
-1.07069360430242));
#11905=CARTESIAN_POINT('Ctrl Pts',(-0.135965654106109,-0.29104845371857,
-1.06788913840721));
#11906=CARTESIAN_POINT('Ctrl Pts',(-0.188025341585962,-0.30527573347708,
-1.05996242598502));
#11907=CARTESIAN_POINT('Ctrl Pts',(-0.214892249704082,-0.308638795020976,
-1.05481642595959));
#11908=CARTESIAN_POINT('Ctrl Pts',(-0.264056468041074,-0.308638795020976,
-1.04359501395068));
#11909=CARTESIAN_POINT('Ctrl Pts',(-0.290495481564827,-0.30527573347708,
-1.036574285215));
#11910=CARTESIAN_POINT('Ctrl Pts',(-0.340838910881557,-0.291048453718569,
-1.02112815447116));
#11911=CARTESIAN_POINT('Ctrl Pts',(-0.364750145543744,-0.28018331644634,
-1.01272583306292));
#11912=CARTESIAN_POINT('Ctrl Pts',(-0.406380688682952,-0.254319232363049,
-0.996771768218699));
#11913=CARTESIAN_POINT('Ctrl Pts',(-0.426157505475872,-0.237895043532788,
-0.988400002689705));
#11914=CARTESIAN_POINT('Ctrl Pts',(-0.460931856495794,-0.199697230012983,
-0.972669835243841));
#11915=CARTESIAN_POINT('Ctrl Pts',(-0.475936279901919,-0.177924977804098,
-0.965323333309091));
#11916=CARTESIAN_POINT('Ctrl Pts',(-0.503136848051454,-0.124911173756694,
-0.951483858396181));
#11917=CARTESIAN_POINT('Ctrl Pts',(-0.513714466572041,-0.0925528133349865,
-0.945684988399766));
#11918=CARTESIAN_POINT('Ctrl Pts',(-0.519393123750572,-0.05953,-0.942555777842682));
#11919=CARTESIAN_POINT('Origin',(-0.244773027351946,-0.05953,-1.07242070340001));
#11920=CARTESIAN_POINT('Origin',(0.,-0.05953,0.));
#11921=CARTESIAN_POINT('',(0.413083465285518,-0.05953,-0.993751811093549));
#11922=CARTESIAN_POINT('Origin',(0.,-0.05953,0.));
#11923=CARTESIAN_POINT('Origin',(0.685838782044607,-0.05953,-0.860014630714833));
#11924=CARTESIAN_POINT('Origin',(0.685838782044607,0.,-0.860014630714833));
#11925=CARTESIAN_POINT('',(0.876916659919095,-0.05953,-0.623857181492959));
#11926=CARTESIAN_POINT('Ctrl Pts',(0.876916659919095,-0.05953,-0.623857181492958));
#11927=CARTESIAN_POINT('Ctrl Pts',(0.873158080166742,-0.0925528133349865,
-0.62914037979579));
#11928=CARTESIAN_POINT('Ctrl Pts',(0.866144010579847,-0.124911173756694,
-0.638954437806245));
#11929=CARTESIAN_POINT('Ctrl Pts',(0.847641868610495,-0.177924977804098,
-0.663225258065736));
#11930=CARTESIAN_POINT('Ctrl Pts',(0.837310877969633,-0.199697230012983,
-0.676354402927683));
#11931=CARTESIAN_POINT('Ctrl Pts',(0.81280533416753,-0.237895043532788,
-0.705614819529209));
#11932=CARTESIAN_POINT('Ctrl Pts',(0.798619410861634,-0.254319232363049,
-0.721738358858166));
#11933=CARTESIAN_POINT('Ctrl Pts',(0.768033796848072,-0.28018331644634,
-0.754175290318038));
#11934=CARTESIAN_POINT('Ctrl Pts',(0.750136149454208,-0.29104845371857,
-0.772120216227122));
#11935=CARTESIAN_POINT('Ctrl Pts',(0.711480111898423,-0.30527573347708,
-0.807879894508811));
#11936=CARTESIAN_POINT('Ctrl Pts',(0.690705563850638,-0.308638795020976,
-0.825676810575913));
#11937=CARTESIAN_POINT('Ctrl Pts',(0.651278921914856,-0.308638795020976,
-0.857118508332695));
#11938=CARTESIAN_POINT('Ctrl Pts',(0.629305439856167,-0.30527573347708,
-0.873412008702649));
#11939=CARTESIAN_POINT('Ctrl Pts',(0.585840553788742,-0.29104845371857,
-0.903141581680914));
#11940=CARTESIAN_POINT('Ctrl Pts',(0.564362943424239,-0.28018331644634,
-0.916597376014514));
#11941=CARTESIAN_POINT('Ctrl Pts',(0.525933334162556,-0.254319232363049,
-0.939198248544427));
#11942=CARTESIAN_POINT('Ctrl Pts',(0.507057380724533,-0.237895043532788,
-0.949440676105255));
#11943=CARTESIAN_POINT('Ctrl Pts',(0.473077587363686,-0.199697230012983,
-0.966820759530997));
#11944=CARTESIAN_POINT('Ctrl Pts',(0.457978755888596,-0.177924977804098,
-0.973971221090534));
#11945=CARTESIAN_POINT('Ctrl Pts',(0.430199341854858,-0.124911173756694,
-0.986608710139579));
#11946=CARTESIAN_POINT('Ctrl Pts',(0.419070565453384,-0.0925528133349865,
-0.991263089003441));
#11947=CARTESIAN_POINT('Ctrl Pts',(0.413083465285518,-0.05953,-0.993751811093549));
#11948=CARTESIAN_POINT('Origin',(0.685838782044607,-0.05953,-0.860014630714833));
#11949=CARTESIAN_POINT('Origin',(0.,-0.208355,0.));
#11950=CARTESIAN_POINT('',(-1.076188,-0.35718,1.31795018948079E-16));
#11951=CARTESIAN_POINT('Origin',(0.,-0.35718,0.));
#11952=CARTESIAN_POINT('',(-1.076188,-0.208355,1.31795018948079E-16));
#11953=CARTESIAN_POINT('',(1.03449977959455,-0.05953,0.296632461748266));
#11954=CARTESIAN_POINT('Origin',(0.,-0.05953,0.));
#11955=CARTESIAN_POINT('',(1.03449977959455,-0.05953,-0.296632461748266));
#11956=CARTESIAN_POINT('Ctrl Pts',(1.03449977959455,-0.05953,0.296632461748267));
#11957=CARTESIAN_POINT('Ctrl Pts',(1.03628691421076,-0.0925528133349865,
0.290399865505497));
#11958=CARTESIAN_POINT('Ctrl Pts',(1.03958665287714,-0.124911173756694,
0.278797079997872));
#11959=CARTESIAN_POINT('Ctrl Pts',(1.0470264474309,-0.177924977804098,0.249198913998601));
#11960=CARTESIAN_POINT('Ctrl Pts',(1.05084995891418,-0.199697230012983,
0.232935932341942));
#11961=CARTESIAN_POINT('Ctrl Pts',(1.05844771715377,-0.237895043532788,
0.195533155353269));
#11962=CARTESIAN_POINT('Ctrl Pts',(1.06220882929878,-0.254319232363049,
0.17438929156337));
#11963=CARTESIAN_POINT('Ctrl Pts',(1.06849922508772,-0.28018331644634,0.130252399648131));
#11964=CARTESIAN_POINT('Ctrl Pts',(1.07137013248666,-0.29104845371857,0.105070977154072));
#11965=CARTESIAN_POINT('Ctrl Pts',(1.07522652957392,-0.30527573347708,0.0525526752791107));
#11966=CARTESIAN_POINT('Ctrl Pts',(1.076188,-0.308638795020976,0.025214283908933));
#11967=CARTESIAN_POINT('Ctrl Pts',(1.076188,-0.308638795020976,-0.025214283908933));
#11968=CARTESIAN_POINT('Ctrl Pts',(1.07522652957392,-0.30527573347708,-0.0525526752791107));
#11969=CARTESIAN_POINT('Ctrl Pts',(1.07137013248666,-0.29104845371857,-0.105070977154072));
#11970=CARTESIAN_POINT('Ctrl Pts',(1.06849922508772,-0.28018331644634,-0.130252399648131));
#11971=CARTESIAN_POINT('Ctrl Pts',(1.06220882929878,-0.254319232363049,
-0.17438929156337));
#11972=CARTESIAN_POINT('Ctrl Pts',(1.05844771715377,-0.237895043532788,
-0.195533155353269));
#11973=CARTESIAN_POINT('Ctrl Pts',(1.05084995891418,-0.199697230012983,
-0.232935932341942));
#11974=CARTESIAN_POINT('Ctrl Pts',(1.0470264474309,-0.177924977804098,-0.249198913998601));
#11975=CARTESIAN_POINT('Ctrl Pts',(1.03958665287714,-0.124911173756694,
-0.278797079997872));
#11976=CARTESIAN_POINT('Ctrl Pts',(1.03628691421076,-0.0925528133349865,
-0.290399865505497));
#11977=CARTESIAN_POINT('Ctrl Pts',(1.03449977959455,-0.05953,-0.296632461748267));
#11978=CARTESIAN_POINT('Origin',(0.,-0.05953,0.));
#11979=CARTESIAN_POINT('Origin',(0.,-0.05953,0.));
#11980=CARTESIAN_POINT('Origin',(1.1,-0.05953,0.));
#11981=CARTESIAN_POINT('Origin',(1.1,0.,0.));
#11982=CARTESIAN_POINT('Origin',(1.1,-0.05953,0.));
#11983=CARTESIAN_POINT('Origin',(0.,-0.35718,0.));
#11984=CARTESIAN_POINT('Origin',(0.,-0.05953,0.));
#11985=CARTESIAN_POINT('',(0.,0.,0.));
#11986=CARTESIAN_POINT('Origin',(1.119765,0.495,0.));
#11987=CARTESIAN_POINT('',(-1.119765,0.495,-1.37131662304724E-16));
#11988=CARTESIAN_POINT('Origin',(0.,0.495,0.));
#11989=CARTESIAN_POINT('',(-1.085235,0.495,-1.32902956907268E-16));
#11990=CARTESIAN_POINT('Origin',(0.,0.495,0.));
#11991=CARTESIAN_POINT('Origin',(0.,0.4575,0.));
#11992=CARTESIAN_POINT('',(-1.119765,0.42,-1.37131662304724E-16));
#11993=CARTESIAN_POINT('Origin',(0.,0.42,0.));
#11994=CARTESIAN_POINT('',(-1.119765,0.4575,-1.37131662304724E-16));
#11995=CARTESIAN_POINT('Origin',(1.085235,0.42,0.));
#11996=CARTESIAN_POINT('',(-1.085235,0.42,-1.32902956907268E-16));
#11997=CARTESIAN_POINT('Origin',(0.,0.42,0.));
#11998=CARTESIAN_POINT('Origin',(0.,0.4575,0.));
#11999=CARTESIAN_POINT('',(-1.085235,0.4575,-1.32902956907268E-16));
#12000=CARTESIAN_POINT('Origin',(1.119765,-0.42,0.));
#12001=CARTESIAN_POINT('',(-1.119765,-0.42,-1.37131662304724E-16));
#12002=CARTESIAN_POINT('Origin',(0.,-0.42,0.));
#12003=CARTESIAN_POINT('',(-1.085235,-0.42,-1.32902956907268E-16));
#12004=CARTESIAN_POINT('Origin',(0.,-0.42,0.));
#12005=CARTESIAN_POINT('Origin',(0.,-0.4575,0.));
#12006=CARTESIAN_POINT('',(-1.119765,-0.495,-1.37131662304724E-16));
#12007=CARTESIAN_POINT('Origin',(0.,-0.495,0.));
#12008=CARTESIAN_POINT('',(-1.119765,-0.4575,-1.37131662304724E-16));
#12009=CARTESIAN_POINT('Origin',(1.085235,-0.495,0.));
#12010=CARTESIAN_POINT('',(-1.085235,-0.495,-1.32902956907268E-16));
#12011=CARTESIAN_POINT('Origin',(0.,-0.495,0.));
#12012=CARTESIAN_POINT('Origin',(0.,-0.4575,0.));
#12013=CARTESIAN_POINT('',(-1.085235,-0.4575,-1.32902956907268E-16));
#12014=CARTESIAN_POINT('',(0.,0.,0.));
#12015=CARTESIAN_POINT('',(0.,0.,0.));
#12016=CARTESIAN_POINT('',(0.,0.,0.));
#12017=CARTESIAN_POINT('',(0.,0.,0.));
#12018=CARTESIAN_POINT('',(0.,0.,0.));
#12019=CARTESIAN_POINT('',(0.,0.,0.));
#12020=CARTESIAN_POINT('Origin',(0.375,0.5,0.));
#12021=CARTESIAN_POINT('',(-0.375,0.5,-4.59242549680257E-17));
#12022=CARTESIAN_POINT('Origin',(0.,0.5,0.));
#12023=CARTESIAN_POINT('Origin',(0.,0.475,0.));
#12024=CARTESIAN_POINT('',(-0.425,0.45,-5.20474889637625E-17));
#12025=CARTESIAN_POINT('Origin',(0.,0.45,0.));
#12026=CARTESIAN_POINT('',(-0.4,0.475,-4.89858719658941E-17));
#12027=CARTESIAN_POINT('Origin',(0.,0.24,0.));
#12028=CARTESIAN_POINT('',(-0.425,0.0299999999999998,-5.20474889637625E-17));
#12029=CARTESIAN_POINT('Origin',(0.,0.0299999999999998,0.));
#12030=CARTESIAN_POINT('',(-0.425,0.24,-5.20474889637625E-17));
#12031=CARTESIAN_POINT('Origin',(0.,0.0150000000000001,0.));
#12032=CARTESIAN_POINT('',(-0.395,4.85722573273506E-17,-4.83735485663204E-17));
#12033=CARTESIAN_POINT('Origin',(0.,0.,0.));
#12034=CARTESIAN_POINT('',(-0.41,0.0150000000000001,-5.02105187650415E-17));
#12035=CARTESIAN_POINT('Origin',(0.27,0.,0.));
#12036=CARTESIAN_POINT('',(-0.27,0.,-3.30654635769785E-17));
#12037=CARTESIAN_POINT('Origin',(0.,0.,0.));
#12038=CARTESIAN_POINT('Origin',(0.,-0.02,0.));
#12039=CARTESIAN_POINT('',(-0.24505,-0.0498999999999999,3.00099698131059E-17));
#12040=CARTESIAN_POINT('Origin',(0.,-0.0498999999999999,0.));
#12041=CARTESIAN_POINT('',(-0.26,-0.02,-3.18408167778312E-17));
#12042=CARTESIAN_POINT('Origin',(0.,-0.995,0.));
#12043=CARTESIAN_POINT('',(-0.24505,-1.95495,3.00099698131059E-17));
#12044=CARTESIAN_POINT('Origin',(0.,-1.95495,0.));
#12045=CARTESIAN_POINT('',(-0.24505,-0.995,-3.00099698131059E-17));
#12046=CARTESIAN_POINT('Origin',(0.,-1.975,0.));
#12047=CARTESIAN_POINT('',(-0.2,-2.,-2.44929359829471E-17));
#12048=CARTESIAN_POINT('Origin',(0.,-2.,0.));
#12049=CARTESIAN_POINT('',(-0.225,-1.975,-2.75545529808154E-17));
#12050=CARTESIAN_POINT('Origin',(0.,-2.,0.));
#12051=CARTESIAN_POINT('Origin',(0.115470053837925,-0.5,-0.2));
#12052=CARTESIAN_POINT('',(0.23094010767585,-0.5,0.));
#12053=CARTESIAN_POINT('',(0.115470053837925,-0.5,-0.2));
#12054=CARTESIAN_POINT('',(0.23094010767585,-0.5,0.));
#12055=CARTESIAN_POINT('',(0.115470053837925,-0.8,-0.2));
#12056=CARTESIAN_POINT('',(0.115470053837925,-0.5,-0.2));
#12057=CARTESIAN_POINT('',(0.23094010767585,-0.8,0.));
#12058=CARTESIAN_POINT('',(0.23094010767585,-0.8,0.));
#12059=CARTESIAN_POINT('',(0.23094010767585,-0.5,0.));
#12060=CARTESIAN_POINT('Origin',(-0.115470053837925,-0.5,-0.2));
#12061=CARTESIAN_POINT('',(-0.115470053837925,-0.5,-0.2));
#12062=CARTESIAN_POINT('',(0.115470053837925,-0.5,-0.2));
#12063=CARTESIAN_POINT('',(-0.115470053837925,-0.8,-0.2));
#12064=CARTESIAN_POINT('',(-0.115470053837925,-0.5,-0.2));
#12065=CARTESIAN_POINT('',(0.115470053837925,-0.8,-0.2));
#12066=CARTESIAN_POINT('Origin',(-0.23094010767585,-0.5,-2.77555756156289E-17));
#12067=CARTESIAN_POINT('',(-0.23094010767585,-0.5,-2.82820063659975E-17));
#12068=CARTESIAN_POINT('',(-0.115470053837925,-0.5,-0.2));
#12069=CARTESIAN_POINT('',(-0.23094010767585,-0.8,-2.77555756156289E-17));
#12070=CARTESIAN_POINT('',(-0.23094010767585,-0.5,-2.82820063659975E-17));
#12071=CARTESIAN_POINT('',(-0.115470053837925,-0.8,-0.2));
#12072=CARTESIAN_POINT('Origin',(-0.115470053837925,-0.5,0.2));
#12073=CARTESIAN_POINT('',(-0.115470053837925,-0.5,0.2));
#12074=CARTESIAN_POINT('',(-0.23094010767585,-0.5,-2.82820063659975E-17));
#12075=CARTESIAN_POINT('',(-0.115470053837925,-0.8,0.2));
#12076=CARTESIAN_POINT('',(-0.115470053837925,-0.5,0.2));
#12077=CARTESIAN_POINT('',(-0.23094010767585,-0.8,-2.82820063659975E-17));
#12078=CARTESIAN_POINT('Origin',(0.115470053837925,-0.5,0.2));
#12079=CARTESIAN_POINT('',(0.115470053837925,-0.5,0.2));
#12080=CARTESIAN_POINT('',(-0.115470053837925,-0.5,0.2));
#12081=CARTESIAN_POINT('',(0.115470053837925,-0.8,0.2));
#12082=CARTESIAN_POINT('',(0.115470053837925,-0.5,0.2));
#12083=CARTESIAN_POINT('',(-0.115470053837925,-0.8,0.2));
#12084=CARTESIAN_POINT('Origin',(0.23094010767585,-0.5,0.));
#12085=CARTESIAN_POINT('',(0.115470053837925,-0.5,0.2));
#12086=CARTESIAN_POINT('',(0.115470053837925,-0.8,0.2));
#12087=CARTESIAN_POINT('Origin',(0.,-0.5,0.));
#12088=CARTESIAN_POINT('Origin',(0.,-0.8,0.));
#12089=CARTESIAN_POINT('',(0.,0.,0.));
#12090=CARTESIAN_POINT('',(0.,0.,0.));
#12091=CARTESIAN_POINT('Origin',(0.75,1.2,0.));
#12092=CARTESIAN_POINT('',(0.885663593019381,1.2,-0.16));
#12093=CARTESIAN_POINT('',(0.885663593019381,1.2,0.16));
#12094=CARTESIAN_POINT('Origin',(0.,1.2,0.));
#12095=CARTESIAN_POINT('',(0.93,1.2,-0.16));
#12096=CARTESIAN_POINT('',(0.93,1.2,-0.16));
#12097=CARTESIAN_POINT('',(0.93,1.2,0.16));
#12098=CARTESIAN_POINT('',(0.93,1.2,0.16));
#12099=CARTESIAN_POINT('',(0.57,1.2,0.16));
#12100=CARTESIAN_POINT('Origin',(0.57,0.,0.16));
#12101=CARTESIAN_POINT('',(0.885663593019381,-1.2,0.16));
#12102=CARTESIAN_POINT('',(0.885663593019381,0.,0.16));
#12103=CARTESIAN_POINT('',(0.93,-1.2,0.16));
#12104=CARTESIAN_POINT('',(0.93,0.,0.16));
#12105=CARTESIAN_POINT('',(0.57,-1.2,0.16));
#12106=CARTESIAN_POINT('Origin',(0.75,-1.2,0.));
#12107=CARTESIAN_POINT('',(0.885663593019381,-1.2,-0.16));
#12108=CARTESIAN_POINT('Origin',(0.,-1.2,0.));
#12109=CARTESIAN_POINT('',(0.93,-1.2,-0.16));
#12110=CARTESIAN_POINT('',(0.93,-1.2,0.16));
#12111=CARTESIAN_POINT('',(0.93,-1.2,-0.16));
#12112=CARTESIAN_POINT('Origin',(0.93,0.,-0.16));
#12113=CARTESIAN_POINT('',(0.885663593019381,0.,-0.16));
#12114=CARTESIAN_POINT('',(0.93,0.,-0.16));
#12115=CARTESIAN_POINT('Origin',(0.93,0.,0.16));
#12116=CARTESIAN_POINT('Origin',(1.05,1.5,0.));
#12117=CARTESIAN_POINT('',(-1.05,1.5,-1.28587913910472E-16));
#12118=CARTESIAN_POINT('Origin',(0.,1.5,0.));
#12119=CARTESIAN_POINT('',(-0.9,1.5,-1.10218211923262E-16));
#12120=CARTESIAN_POINT('Origin',(0.,1.5,0.));
#12121=CARTESIAN_POINT('Origin',(0.,1.315,0.));
#12122=CARTESIAN_POINT('',(-1.05,1.13,-1.28587913910472E-16));
#12123=CARTESIAN_POINT('Origin',(0.,1.13,0.));
#12124=CARTESIAN_POINT('',(-1.05,1.315,-1.28587913910472E-16));
#12125=CARTESIAN_POINT('Origin',(1.,1.13,0.));
#12126=CARTESIAN_POINT('',(-1.,1.13,-1.22464679914735E-16));
#12127=CARTESIAN_POINT('Origin',(0.,1.13,0.));
#12128=CARTESIAN_POINT('Origin',(0.,1.065,0.));
#12129=CARTESIAN_POINT('',(-1.,1.,-1.22464679914735E-16));
#12130=CARTESIAN_POINT('Origin',(0.,1.,0.));
#12131=CARTESIAN_POINT('',(-1.,1.065,-1.22464679914735E-16));
#12132=CARTESIAN_POINT('Origin',(1.05,1.,0.));
#12133=CARTESIAN_POINT('',(-1.05,1.,-1.28587913910472E-16));
#12134=CARTESIAN_POINT('Origin',(0.,1.,0.));
#12135=CARTESIAN_POINT('Origin',(0.,0.,0.));
#12136=CARTESIAN_POINT('',(-1.05,-1.,-1.28587913910472E-16));
#12137=CARTESIAN_POINT('Origin',(0.,-1.,0.));
#12138=CARTESIAN_POINT('',(-1.05,0.,-1.28587913910472E-16));
#12139=CARTESIAN_POINT('Origin',(1.,-1.,0.));
#12140=CARTESIAN_POINT('',(-1.,-1.,-1.22464679914735E-16));
#12141=CARTESIAN_POINT('Origin',(0.,-1.,0.));
#12142=CARTESIAN_POINT('Origin',(0.,-1.065,0.));
#12143=CARTESIAN_POINT('',(-1.,-1.13,-1.22464679914735E-16));
#12144=CARTESIAN_POINT('Origin',(0.,-1.13,0.));
#12145=CARTESIAN_POINT('',(-1.,-1.065,-1.22464679914735E-16));
#12146=CARTESIAN_POINT('Origin',(1.05,-1.13,0.));
#12147=CARTESIAN_POINT('',(-1.05,-1.13,-1.28587913910472E-16));
#12148=CARTESIAN_POINT('Origin',(0.,-1.13,0.));
#12149=CARTESIAN_POINT('Origin',(0.,-1.315,0.));
#12150=CARTESIAN_POINT('',(-1.05,-1.5,-1.28587913910472E-16));
#12151=CARTESIAN_POINT('Origin',(0.,-1.5,0.));
#12152=CARTESIAN_POINT('',(-1.05,-1.315,-1.28587913910472E-16));
#12153=CARTESIAN_POINT('Origin',(0.9,-1.5,0.));
#12154=CARTESIAN_POINT('',(-0.9,-1.5,-1.10218211923262E-16));
#12155=CARTESIAN_POINT('Origin',(0.,-1.5,0.));
#12156=CARTESIAN_POINT('Origin',(0.,0.,0.));
#12157=CARTESIAN_POINT('',(-0.9,0.,-1.10218211923262E-16));
#12158=CARTESIAN_POINT('',(0.,0.,0.));
#12159=CARTESIAN_POINT('Origin',(0.75,1.2,0.));
#12160=CARTESIAN_POINT('',(0.880582193778639,1.2,0.16));
#12161=CARTESIAN_POINT('',(0.880582193778639,1.2,-0.16));
#12162=CARTESIAN_POINT('Origin',(0.,1.2,0.));
#12163=CARTESIAN_POINT('',(0.583459510163302,1.2,0.16));
#12164=CARTESIAN_POINT('',(0.57,1.2,0.16));
#12165=CARTESIAN_POINT('',(0.583459510163302,1.2,-0.16));
#12166=CARTESIAN_POINT('Origin',(0.,1.2,0.));
#12167=CARTESIAN_POINT('',(0.93,1.2,-0.16));
#12168=CARTESIAN_POINT('Origin',(0.93,0.,-0.16));
#12169=CARTESIAN_POINT('',(0.880582193778639,-1.2,-0.16));
#12170=CARTESIAN_POINT('',(0.880582193778639,0.,-0.16));
#12171=CARTESIAN_POINT('',(0.583459510163302,-1.2,-0.16));
#12172=CARTESIAN_POINT('',(0.583459510163302,0.,-0.16));
#12173=CARTESIAN_POINT('',(0.93,-1.2,-0.16));
#12174=CARTESIAN_POINT('Origin',(0.75,-1.2,0.));
#12175=CARTESIAN_POINT('',(0.880582193778639,-1.2,0.16));
#12176=CARTESIAN_POINT('Origin',(0.,-1.2,0.));
#12177=CARTESIAN_POINT('',(0.583459510163302,-1.2,0.16));
#12178=CARTESIAN_POINT('Origin',(0.,-1.2,0.));
#12179=CARTESIAN_POINT('',(0.57,-1.2,0.16));
#12180=CARTESIAN_POINT('Origin',(0.57,0.,0.16));
#12181=CARTESIAN_POINT('',(0.880582193778639,0.,0.16));
#12182=CARTESIAN_POINT('',(0.583459510163302,0.,0.16));
#12183=CARTESIAN_POINT('Origin',(0.895,1.35,0.));
#12184=CARTESIAN_POINT('',(-0.895,1.35,-1.09605888523688E-16));
#12185=CARTESIAN_POINT('Origin',(0.,1.35,0.));
#12186=CARTESIAN_POINT('',(-0.605,1.35,-7.40911313484149E-17));
#12187=CARTESIAN_POINT('Origin',(0.,1.35,0.));
#12188=CARTESIAN_POINT('Origin',(0.,0.,0.));
#12189=CARTESIAN_POINT('',(-0.895,-1.35,-1.09605888523688E-16));
#12190=CARTESIAN_POINT('Origin',(0.,-1.35,0.));
#12191=CARTESIAN_POINT('',(-0.895,0.,-1.09605888523688E-16));
#12192=CARTESIAN_POINT('Origin',(0.605,-1.35,0.));
#12193=CARTESIAN_POINT('',(-0.605,-1.35,-7.40911313484149E-17));
#12194=CARTESIAN_POINT('Origin',(0.,-1.35,0.));
#12195=CARTESIAN_POINT('Origin',(0.,0.,0.));
#12196=CARTESIAN_POINT('',(-0.605,0.,-7.40911313484149E-17));
#12197=CARTESIAN_POINT('',(0.,0.,0.));
#12198=CARTESIAN_POINT('',(0.,0.,0.));
#12199=CARTESIAN_POINT('',(0.,0.,0.));
#12200=CARTESIAN_POINT('Origin',(0.0866025403784439,-0.4,-0.15));
#12201=CARTESIAN_POINT('',(0.173205080756888,-0.4,0.));
#12202=CARTESIAN_POINT('',(0.0866025403784439,-0.4,-0.15));
#12203=CARTESIAN_POINT('',(0.173205080756888,-0.4,0.));
#12204=CARTESIAN_POINT('',(0.0866025403784439,-0.64,-0.15));
#12205=CARTESIAN_POINT('',(0.0866025403784439,-0.4,-0.15));
#12206=CARTESIAN_POINT('',(0.173205080756888,-0.64,0.));
#12207=CARTESIAN_POINT('',(0.173205080756888,-0.64,0.));
#12208=CARTESIAN_POINT('',(0.173205080756888,-0.4,0.));
#12209=CARTESIAN_POINT('Origin',(-0.0866025403784438,-0.4,-0.15));
#12210=CARTESIAN_POINT('',(-0.0866025403784438,-0.4,-0.15));
#12211=CARTESIAN_POINT('',(0.0866025403784439,-0.4,-0.15));
#12212=CARTESIAN_POINT('',(-0.0866025403784438,-0.64,-0.15));
#12213=CARTESIAN_POINT('',(-0.0866025403784438,-0.4,-0.15));
#12214=CARTESIAN_POINT('',(0.0866025403784439,-0.64,-0.15));
#12215=CARTESIAN_POINT('Origin',(-0.173205080756888,-0.4,-2.77555756156289E-17));
#12216=CARTESIAN_POINT('',(-0.173205080756888,-0.4,-2.12115047744981E-17));
#12217=CARTESIAN_POINT('',(-0.0866025403784438,-0.4,-0.15));
#12218=CARTESIAN_POINT('',(-0.173205080756888,-0.64,-2.77555756156289E-17));
#12219=CARTESIAN_POINT('',(-0.173205080756888,-0.4,-2.12115047744981E-17));
#12220=CARTESIAN_POINT('',(-0.0866025403784438,-0.64,-0.15));
#12221=CARTESIAN_POINT('Origin',(-0.0866025403784439,-0.4,0.15));
#12222=CARTESIAN_POINT('',(-0.0866025403784439,-0.4,0.15));
#12223=CARTESIAN_POINT('',(-0.173205080756888,-0.4,-2.12115047744981E-17));
#12224=CARTESIAN_POINT('',(-0.0866025403784439,-0.64,0.15));
#12225=CARTESIAN_POINT('',(-0.0866025403784439,-0.4,0.15));
#12226=CARTESIAN_POINT('',(-0.173205080756888,-0.64,-2.12115047744981E-17));
#12227=CARTESIAN_POINT('Origin',(0.0866025403784439,-0.4,0.15));
#12228=CARTESIAN_POINT('',(0.0866025403784439,-0.4,0.15));
#12229=CARTESIAN_POINT('',(-0.0866025403784439,-0.4,0.15));
#12230=CARTESIAN_POINT('',(0.0866025403784439,-0.64,0.15));
#12231=CARTESIAN_POINT('',(0.0866025403784439,-0.4,0.15));
#12232=CARTESIAN_POINT('',(-0.0866025403784439,-0.64,0.15));
#12233=CARTESIAN_POINT('Origin',(0.173205080756888,-0.4,0.));
#12234=CARTESIAN_POINT('',(0.0866025403784439,-0.4,0.15));
#12235=CARTESIAN_POINT('',(0.0866025403784439,-0.64,0.15));
#12236=CARTESIAN_POINT('Origin',(0.,-0.4,-2.77555756156289E-17));
#12237=CARTESIAN_POINT('Origin',(0.,-0.64,-2.77555756156289E-17));
#12238=CARTESIAN_POINT('Origin',(0.,-1.,0.));
#12239=CARTESIAN_POINT('',(-0.1954,-1.,2.39295984553393E-17));
#12240=CARTESIAN_POINT('Origin',(0.,-1.,0.));
#12241=CARTESIAN_POINT('Origin',(0.3,0.4,0.));
#12242=CARTESIAN_POINT('',(-0.3,0.4,-3.67394039744206E-17));
#12243=CARTESIAN_POINT('Origin',(0.,0.4,0.));
#12244=CARTESIAN_POINT('Origin',(0.,0.375,0.));
#12245=CARTESIAN_POINT('',(-0.35,0.35,-4.28626379701573E-17));
#12246=CARTESIAN_POINT('Origin',(0.,0.35,0.));
#12247=CARTESIAN_POINT('',(-0.325,0.375,-3.9801020972289E-17));
#12248=CARTESIAN_POINT('Origin',(0.,0.19,0.));
#12249=CARTESIAN_POINT('',(-0.35,0.03,-4.28626379701574E-17));
#12250=CARTESIAN_POINT('Origin',(0.,0.03,0.));
#12251=CARTESIAN_POINT('',(-0.35,0.19,-4.28626379701574E-17));
#12252=CARTESIAN_POINT('Origin',(0.,0.0149999999999999,0.));
#12253=CARTESIAN_POINT('',(-0.32,-3.29597460435593E-17,-3.91886975727153E-17));
#12254=CARTESIAN_POINT('Origin',(0.,0.,0.));
#12255=CARTESIAN_POINT('',(-0.335,0.0149999999999999,-4.10256677714363E-17));
#12256=CARTESIAN_POINT('Origin',(0.22,0.,0.));
#12257=CARTESIAN_POINT('',(-0.22,-6.93889390390723E-18,-2.69422295812418E-17));
#12258=CARTESIAN_POINT('Origin',(0.,0.,0.));
#12259=CARTESIAN_POINT('Origin',(0.,-0.02,0.));
#12260=CARTESIAN_POINT('',(-0.1954,-0.0492,2.39295984553393E-17));
#12261=CARTESIAN_POINT('Origin',(0.,-0.0492,0.));
#12262=CARTESIAN_POINT('',(-0.21,-0.02,-2.57175827820944E-17));
#12263=CARTESIAN_POINT('Origin',(0.,-0.8,0.));
#12264=CARTESIAN_POINT('',(-0.1954,-0.8,-2.39295984553393E-17));
#12265=CARTESIAN_POINT('',(0.,0.,0.));
#12266=CARTESIAN_POINT('',(0.,0.,0.));
#12267=CARTESIAN_POINT('Origin',(0.,5.,4.));
#12268=CARTESIAN_POINT('',(-0.165,5.,4.));
#12269=CARTESIAN_POINT('Origin',(0.,5.,4.));
#12270=CARTESIAN_POINT('',(-0.165,6.5,4.));
#12271=CARTESIAN_POINT('',(-0.165,5.,4.));
#12272=CARTESIAN_POINT('Origin',(0.,6.5,4.));
#12273=CARTESIAN_POINT('Origin',(0.,5.,4.));
#12274=CARTESIAN_POINT('Origin',(0.,-4.6,4.));
#12275=CARTESIAN_POINT('',(-0.165,-4.5,4.));
#12276=CARTESIAN_POINT('Origin',(0.,-4.5,4.));
#12277=CARTESIAN_POINT('',(-0.165,-2.9,4.));
#12278=CARTESIAN_POINT('',(-0.165,-4.6,4.));
#12279=CARTESIAN_POINT('Origin',(0.,-2.9,4.));
#12280=CARTESIAN_POINT('Origin',(0.,-2.9,4.));
#12281=CARTESIAN_POINT('Origin',(-0.2,4.8,3.3));
#12282=CARTESIAN_POINT('',(-0.2,6.2,3.43431457505076));
#12283=CARTESIAN_POINT('',(-0.2,4.8,3.43431457505076));
#12284=CARTESIAN_POINT('',(-0.2,-4.5,3.43431457505076));
#12285=CARTESIAN_POINT('',(-0.2,6.2,3.65));
#12286=CARTESIAN_POINT('',(-0.2,6.2,3.65));
#12287=CARTESIAN_POINT('',(-0.2,4.8,3.65));
#12288=CARTESIAN_POINT('',(-0.2,4.8,3.65));
#12289=CARTESIAN_POINT('',(-0.2,4.8,3.65));
#12290=CARTESIAN_POINT('Origin',(0.,4.8,3.475));
#12291=CARTESIAN_POINT('',(0.2,4.8,3.43431457505076));
#12292=CARTESIAN_POINT('Origin',(0.,4.8,4.));
#12293=CARTESIAN_POINT('',(0.2,4.8,3.65));
#12294=CARTESIAN_POINT('',(0.2,4.8,3.65));
#12295=CARTESIAN_POINT('',(0.2,4.8,3.3));
#12296=CARTESIAN_POINT('Origin',(0.2,4.8,3.65));
#12297=CARTESIAN_POINT('',(0.2,6.2,3.43431457505076));
#12298=CARTESIAN_POINT('',(0.2,-4.5,3.43431457505076));
#12299=CARTESIAN_POINT('',(0.2,6.2,3.65));
#12300=CARTESIAN_POINT('',(0.2,4.8,3.65));
#12301=CARTESIAN_POINT('',(0.2,6.2,3.3));
#12302=CARTESIAN_POINT('Origin',(-0.2,4.8,3.65));
#12303=CARTESIAN_POINT('',(0.2,6.2,3.65));
#12304=CARTESIAN_POINT('Origin',(0.,6.2,3.475));
#12305=CARTESIAN_POINT('Origin',(0.,6.2,4.));
#12306=CARTESIAN_POINT('Origin',(-0.2,-0.7,3.3));
#12307=CARTESIAN_POINT('',(-0.2,0.7,3.43431457505076));
#12308=CARTESIAN_POINT('',(-0.2,-0.7,3.43431457505076));
#12309=CARTESIAN_POINT('',(-0.2,-4.5,3.43431457505076));
#12310=CARTESIAN_POINT('',(-0.2,0.7,3.65));
#12311=CARTESIAN_POINT('',(-0.2,0.7,3.65));
#12312=CARTESIAN_POINT('',(-0.2,-0.7,3.65));
#12313=CARTESIAN_POINT('',(-0.2,-0.7,3.65));
#12314=CARTESIAN_POINT('',(-0.2,-0.7,3.65));
#12315=CARTESIAN_POINT('Origin',(0.,-0.7,3.475));
#12316=CARTESIAN_POINT('',(0.2,-0.7,3.43431457505076));
#12317=CARTESIAN_POINT('Origin',(0.,-0.7,4.));
#12318=CARTESIAN_POINT('',(0.2,-0.7,3.65));
#12319=CARTESIAN_POINT('',(0.2,-0.7,3.65));
#12320=CARTESIAN_POINT('',(0.2,-0.7,3.3));
#12321=CARTESIAN_POINT('Origin',(0.2,-0.7,3.65));
#12322=CARTESIAN_POINT('',(0.2,0.7,3.43431457505076));
#12323=CARTESIAN_POINT('',(0.2,-4.5,3.43431457505076));
#12324=CARTESIAN_POINT('',(0.2,0.7,3.65));
#12325=CARTESIAN_POINT('',(0.2,-0.7,3.65));
#12326=CARTESIAN_POINT('',(0.2,0.7,3.3));
#12327=CARTESIAN_POINT('Origin',(-0.2,-0.7,3.65));
#12328=CARTESIAN_POINT('',(0.2,0.7,3.65));
#12329=CARTESIAN_POINT('Origin',(0.,0.7,3.475));
#12330=CARTESIAN_POINT('Origin',(0.,0.7,4.));
#12331=CARTESIAN_POINT('Origin',(0.,-4.5,4.));
#12332=CARTESIAN_POINT('',(-0.6,6.5,4.));
#12333=CARTESIAN_POINT('Origin',(0.,6.5,4.));
#12334=CARTESIAN_POINT('',(-0.6,-4.5,4.));
#12335=CARTESIAN_POINT('',(-0.6,-4.5,4.));
#12336=CARTESIAN_POINT('Origin',(0.,-4.5,4.));
#12337=CARTESIAN_POINT('Origin',(0.,6.5,4.));
#12338=CARTESIAN_POINT('Origin',(0.,-4.5,4.));
#12339=CARTESIAN_POINT('',(0.,0.,0.));
#12340=CARTESIAN_POINT('Origin',(0.,-2.,4.));
#12341=CARTESIAN_POINT('',(-0.605,-1.,4.));
#12342=CARTESIAN_POINT('Origin',(0.,-1.,4.));
#12343=CARTESIAN_POINT('',(-0.605,-2.,4.));
#12344=CARTESIAN_POINT('',(-0.605,-2.,4.));
#12345=CARTESIAN_POINT('Origin',(0.,-2.,4.));
#12346=CARTESIAN_POINT('Origin',(0.,-2.,4.));
#12347=CARTESIAN_POINT('',(-0.8,-1.,4.));
#12348=CARTESIAN_POINT('Origin',(0.,-1.,4.));
#12349=CARTESIAN_POINT('',(-0.8,-2.,4.));
#12350=CARTESIAN_POINT('',(-0.8,-2.,4.));
#12351=CARTESIAN_POINT('Origin',(0.,-2.,4.));
#12352=CARTESIAN_POINT('Origin',(0.,-1.,4.));
#12353=CARTESIAN_POINT('Origin',(0.,-2.,4.));
#12354=CARTESIAN_POINT('',(0.,0.,0.));
#12355=CARTESIAN_POINT('Origin',(0.,1.,4.));
#12356=CARTESIAN_POINT('',(-0.605,2.,4.));
#12357=CARTESIAN_POINT('Origin',(0.,2.,4.));
#12358=CARTESIAN_POINT('',(-0.605,1.,4.));
#12359=CARTESIAN_POINT('',(-0.605,1.,4.));
#12360=CARTESIAN_POINT('Origin',(0.,1.,4.));
#12361=CARTESIAN_POINT('Origin',(0.,1.,4.));
#12362=CARTESIAN_POINT('',(-0.8,2.,4.));
#12363=CARTESIAN_POINT('Origin',(0.,2.,4.));
#12364=CARTESIAN_POINT('',(-0.8,1.,4.));
#12365=CARTESIAN_POINT('',(-0.8,1.,4.));
#12366=CARTESIAN_POINT('Origin',(0.,1.,4.));
#12367=CARTESIAN_POINT('Origin',(0.,2.,4.));
#12368=CARTESIAN_POINT('Origin',(0.,1.,4.));
#12369=CARTESIAN_POINT('',(0.,0.,0.));
#12370=CARTESIAN_POINT('Origin',(0.,-4.5,4.));
#12371=CARTESIAN_POINT('',(-0.605,-3.,4.));
#12372=CARTESIAN_POINT('Origin',(0.,-3.,4.));
#12373=CARTESIAN_POINT('',(-0.605,-4.5,4.));
#12374=CARTESIAN_POINT('',(-0.605,-4.5,4.));
#12375=CARTESIAN_POINT('Origin',(0.,-4.5,4.));
#12376=CARTESIAN_POINT('Origin',(0.,-4.5,4.));
#12377=CARTESIAN_POINT('',(-0.8,-3.,4.));
#12378=CARTESIAN_POINT('Origin',(0.,-3.,4.));
#12379=CARTESIAN_POINT('',(-0.8,-4.5,4.));
#12380=CARTESIAN_POINT('',(-0.8,-4.5,4.));
#12381=CARTESIAN_POINT('Origin',(0.,-4.5,4.));
#12382=CARTESIAN_POINT('Origin',(0.,-3.,4.));
#12383=CARTESIAN_POINT('Origin',(0.,-4.5,4.));
#12384=CARTESIAN_POINT('',(0.,0.,0.));
#12385=CARTESIAN_POINT('Origin',(0.,3.,4.));
#12386=CARTESIAN_POINT('',(-0.605,4.5,4.));
#12387=CARTESIAN_POINT('Origin',(0.,4.5,4.));
#12388=CARTESIAN_POINT('',(-0.605,3.,4.));
#12389=CARTESIAN_POINT('',(-0.605,3.,4.));
#12390=CARTESIAN_POINT('Origin',(0.,3.,4.));
#12391=CARTESIAN_POINT('Origin',(0.,3.,4.));
#12392=CARTESIAN_POINT('',(-0.8,4.5,4.));
#12393=CARTESIAN_POINT('Origin',(0.,4.5,4.));
#12394=CARTESIAN_POINT('',(-0.8,3.,4.));
#12395=CARTESIAN_POINT('',(-0.8,3.,4.));
#12396=CARTESIAN_POINT('Origin',(0.,3.,4.));
#12397=CARTESIAN_POINT('Origin',(0.,4.5,4.));
#12398=CARTESIAN_POINT('Origin',(0.,3.,4.));
#12399=CARTESIAN_POINT('',(0.,0.,0.));
#12400=CARTESIAN_POINT('Origin',(-0.2,-1.1,3.22));
#12401=CARTESIAN_POINT('',(-0.2,-1.,3.22));
#12402=CARTESIAN_POINT('',(-0.2,-1.,3.43431457505076));
#12403=CARTESIAN_POINT('',(-0.2,-1.,3.61));
#12404=CARTESIAN_POINT('',(-0.2,1.,3.22));
#12405=CARTESIAN_POINT('',(-0.2,-1.1,3.22));
#12406=CARTESIAN_POINT('',(-0.2,1.,3.43431457505076));
#12407=CARTESIAN_POINT('',(-0.2,1.,3.61));
#12408=CARTESIAN_POINT('',(-0.2,-1.1,3.43431457505076));
#12409=CARTESIAN_POINT('Origin',(0.2,-1.1,3.22));
#12410=CARTESIAN_POINT('',(0.2,-1.,3.22));
#12411=CARTESIAN_POINT('',(0.1,-1.,3.22));
#12412=CARTESIAN_POINT('',(0.2,1.,3.22));
#12413=CARTESIAN_POINT('',(0.2,-1.1,3.22));
#12414=CARTESIAN_POINT('',(0.1,1.,3.22));
#12415=CARTESIAN_POINT('Origin',(0.2,-1.1,4.));
#12416=CARTESIAN_POINT('',(0.2,-1.,3.43431457505076));
#12417=CARTESIAN_POINT('',(0.2,-1.,4.));
#12418=CARTESIAN_POINT('',(0.2,1.,3.43431457505076));
#12419=CARTESIAN_POINT('',(0.2,-1.1,3.43431457505076));
#12420=CARTESIAN_POINT('',(0.2,1.,4.));
#12421=CARTESIAN_POINT('Origin',(0.,1.,4.));
#12422=CARTESIAN_POINT('',(-1.2,1.,4.));
#12423=CARTESIAN_POINT('Origin',(0.,1.,4.));
#12424=CARTESIAN_POINT('Origin',(0.,1.,4.));
#12425=CARTESIAN_POINT('Origin',(0.,-1.1,4.));
#12426=CARTESIAN_POINT('Origin',(0.,-1.,4.));
#12427=CARTESIAN_POINT('Origin',(0.,-1.,4.));
#12428=CARTESIAN_POINT('',(-1.2,-0.6,4.));
#12429=CARTESIAN_POINT('Origin',(0.,-0.6,4.));
#12430=CARTESIAN_POINT('',(-1.2,-1.,4.));
#12431=CARTESIAN_POINT('',(-1.2,-1.,4.));
#12432=CARTESIAN_POINT('Origin',(0.,-1.,4.));
#12433=CARTESIAN_POINT('Origin',(0.,-1.,4.));
#12434=CARTESIAN_POINT('',(-1.2,0.6,4.));
#12435=CARTESIAN_POINT('',(-1.2,-1.,4.));
#12436=CARTESIAN_POINT('Origin',(0.,0.6,4.));
#12437=CARTESIAN_POINT('Origin',(0.,-1.,4.));
#12438=CARTESIAN_POINT('Origin',(0.,-0.6,4.4));
#12439=CARTESIAN_POINT('',(-2.,0.6,4.4));
#12440=CARTESIAN_POINT('Origin',(0.,0.6,4.4));
#12441=CARTESIAN_POINT('',(-2.,-0.6,4.4));
#12442=CARTESIAN_POINT('',(-2.,-0.6,4.4));
#12443=CARTESIAN_POINT('Origin',(0.,-0.6,4.4));
#12444=CARTESIAN_POINT('Origin',(0.,0.6,4.4));
#12445=CARTESIAN_POINT('Origin',(0.,-0.6,4.4));
#12446=CARTESIAN_POINT('',(0.,0.,0.));
#12447=CARTESIAN_POINT('Origin',(2.5,4.9,4.));
#12448=CARTESIAN_POINT('',(2.275,5.,4.));
#12449=CARTESIAN_POINT('Origin',(2.5,5.,4.));
#12450=CARTESIAN_POINT('',(2.275,5.8,4.));
#12451=CARTESIAN_POINT('',(2.275,4.9,4.));
#12452=CARTESIAN_POINT('Origin',(2.5,5.8,4.));
#12453=CARTESIAN_POINT('Origin',(-0.2,4.4,3.22));
#12454=CARTESIAN_POINT('',(-0.2,4.5,3.22));
#12455=CARTESIAN_POINT('',(-0.2,4.5,3.43431457505076));
#12456=CARTESIAN_POINT('',(-0.2,4.5,3.61));
#12457=CARTESIAN_POINT('',(-0.2,6.5,3.22));
#12458=CARTESIAN_POINT('',(-0.2,4.4,3.22));
#12459=CARTESIAN_POINT('',(-0.2,6.5,3.43431457505076));
#12460=CARTESIAN_POINT('',(-0.2,6.5,3.61));
#12461=CARTESIAN_POINT('',(-0.2,4.5,3.43431457505076));
#12462=CARTESIAN_POINT('Origin',(0.2,4.4,3.22));
#12463=CARTESIAN_POINT('',(0.2,4.5,3.22));
#12464=CARTESIAN_POINT('',(0.1,4.5,3.22));
#12465=CARTESIAN_POINT('',(0.2,6.5,3.22));
#12466=CARTESIAN_POINT('',(0.2,4.4,3.22));
#12467=CARTESIAN_POINT('',(0.1,6.5,3.22));
#12468=CARTESIAN_POINT('Origin',(0.2,4.4,4.));
#12469=CARTESIAN_POINT('',(0.2,4.5,3.43431457505076));
#12470=CARTESIAN_POINT('',(0.2,4.5,4.));
#12471=CARTESIAN_POINT('',(0.2,6.5,3.43431457505076));
#12472=CARTESIAN_POINT('',(0.2,4.5,3.43431457505076));
#12473=CARTESIAN_POINT('',(0.2,6.5,4.));
#12474=CARTESIAN_POINT('Origin',(0.,6.5,4.));
#12475=CARTESIAN_POINT('',(-1.2,6.5,4.));
#12476=CARTESIAN_POINT('Origin',(0.,6.5,4.));
#12477=CARTESIAN_POINT('Origin',(0.,6.5,4.));
#12478=CARTESIAN_POINT('Origin',(0.,4.5,4.));
#12479=CARTESIAN_POINT('Origin',(0.,4.5,4.));
#12480=CARTESIAN_POINT('Origin',(2.5,5.,4.));
#12481=CARTESIAN_POINT('',(1.9255437353462,5.8,3.6));
#12482=CARTESIAN_POINT('',(1.9255437353462,5.,3.6));
#12483=CARTESIAN_POINT('',(1.9255437353462,5.,3.6));
#12484=CARTESIAN_POINT('',(1.9255437353462,5.8,4.4));
#12485=CARTESIAN_POINT('Origin',(2.5,5.8,4.));
#12486=CARTESIAN_POINT('',(1.9255437353462,5.,4.4));
#12487=CARTESIAN_POINT('',(1.9255437353462,5.,4.4));
#12488=CARTESIAN_POINT('Origin',(2.5,5.,4.));
#12489=CARTESIAN_POINT('Origin',(1.25,5.,4.));
#12490=CARTESIAN_POINT('',(1.13137084989848,5.,4.4));
#12491=CARTESIAN_POINT('',(2.5,5.,4.4));
#12492=CARTESIAN_POINT('',(1.13137084989848,5.,3.6));
#12493=CARTESIAN_POINT('Origin',(0.,5.,4.));
#12494=CARTESIAN_POINT('',(0.,5.,3.6));
#12495=CARTESIAN_POINT('Origin',(0.,5.,4.4));
#12496=CARTESIAN_POINT('',(1.13137084989848,5.8,4.4));
#12497=CARTESIAN_POINT('',(2.5,5.8,4.4));
#12498=CARTESIAN_POINT('',(1.13137084989848,4.5,4.4));
#12499=CARTESIAN_POINT('Origin',(2.5,5.,3.6));
#12500=CARTESIAN_POINT('',(1.13137084989848,5.8,3.6));
#12501=CARTESIAN_POINT('',(1.13137084989848,4.5,3.6));
#12502=CARTESIAN_POINT('',(0.,5.8,3.6));
#12503=CARTESIAN_POINT('Origin',(1.25,5.8,4.));
#12504=CARTESIAN_POINT('Origin',(0.,5.8,4.));
#12505=CARTESIAN_POINT('Origin',(0.,4.5,4.));
#12506=CARTESIAN_POINT('',(-1.2,4.5,4.));
#12507=CARTESIAN_POINT('',(-1.2,4.5,4.));
#12508=CARTESIAN_POINT('Origin',(0.,4.5,4.));
#12509=CARTESIAN_POINT('Origin',(0.,4.5,4.));
#12510=CARTESIAN_POINT('',(0.,0.,0.));
#12511=CARTESIAN_POINT('Origin',(2.5,5.7,4.));
#12512=CARTESIAN_POINT('',(2.335,5.8,4.));
#12513=CARTESIAN_POINT('Origin',(2.5,5.8,4.));
#12514=CARTESIAN_POINT('',(2.335,6.9,4.));
#12515=CARTESIAN_POINT('',(2.335,5.7,4.));
#12516=CARTESIAN_POINT('Origin',(2.5,6.9,4.));
#12517=CARTESIAN_POINT('Origin',(2.5,6.9,4.));
#12518=CARTESIAN_POINT('Origin',(2.5,5.8,4.));
#12519=CARTESIAN_POINT('',(1.9,8.2,4.));
#12520=CARTESIAN_POINT('Origin',(2.5,8.2,4.));
#12521=CARTESIAN_POINT('',(1.9,5.8,4.));
#12522=CARTESIAN_POINT('',(1.9,5.8,4.));
#12523=CARTESIAN_POINT('Origin',(2.5,5.8,4.));
#12524=CARTESIAN_POINT('Origin',(2.5,8.2,4.));
#12525=CARTESIAN_POINT('Origin',(2.5,5.8,4.));
#12526=CARTESIAN_POINT('',(0.,0.,0.));
#12527=CARTESIAN_POINT('Origin',(0.,-4.7,4.));
#12528=CARTESIAN_POINT('',(-0.225,-4.5,4.));
#12529=CARTESIAN_POINT('Origin',(0.,-4.5,4.));
#12530=CARTESIAN_POINT('',(-0.225,-4.7,4.));
#12531=CARTESIAN_POINT('',(-0.225,-4.7,4.));
#12532=CARTESIAN_POINT('Origin',(0.,-4.7,4.));
#12533=CARTESIAN_POINT('Origin',(0.,-4.7,4.));
#12534=CARTESIAN_POINT('',(-1.,-4.5,4.));
#12535=CARTESIAN_POINT('Origin',(0.,-4.5,4.));
#12536=CARTESIAN_POINT('',(-1.,-4.7,4.));
#12537=CARTESIAN_POINT('',(-1.,-4.7,4.));
#12538=CARTESIAN_POINT('Origin',(0.,-4.7,4.));
#12539=CARTESIAN_POINT('Origin',(0.,-4.5,4.));
#12540=CARTESIAN_POINT('Origin',(0.,-4.7,4.));
#12541=CARTESIAN_POINT('',(0.,0.,0.));
#12542=CARTESIAN_POINT('Origin',(0.,6.5,4.));
#12543=CARTESIAN_POINT('',(-0.225,6.7,4.));
#12544=CARTESIAN_POINT('Origin',(0.,6.7,4.));
#12545=CARTESIAN_POINT('',(-0.225,6.5,4.));
#12546=CARTESIAN_POINT('',(-0.225,6.5,4.));
#12547=CARTESIAN_POINT('Origin',(0.,6.5,4.));
#12548=CARTESIAN_POINT('Origin',(0.,6.5,4.));
#12549=CARTESIAN_POINT('',(-1.,6.7,4.));
#12550=CARTESIAN_POINT('Origin',(0.,6.7,4.));
#12551=CARTESIAN_POINT('',(-1.,6.5,4.));
#12552=CARTESIAN_POINT('',(-1.,6.5,4.));
#12553=CARTESIAN_POINT('Origin',(0.,6.5,4.));
#12554=CARTESIAN_POINT('Origin',(0.,6.7,4.));
#12555=CARTESIAN_POINT('Origin',(0.,6.5,4.));
#12556=CARTESIAN_POINT('',(0.,0.,0.));
#12557=CARTESIAN_POINT('Origin',(0.7,0.,0.25));
#12558=CARTESIAN_POINT('',(0.7,0.16,0.4));
#12559=CARTESIAN_POINT('',(0.7,0.2,0.36));
#12560=CARTESIAN_POINT('',(0.7,0.1675,0.3925));
#12561=CARTESIAN_POINT('',(0.7,-0.16,0.4));
#12562=CARTESIAN_POINT('',(0.7,0.,0.4));
#12563=CARTESIAN_POINT('',(0.7,-0.2,0.36));
#12564=CARTESIAN_POINT('',(0.7,-0.1675,0.3925));
#12565=CARTESIAN_POINT('',(0.7,-0.2,0.04));
#12566=CARTESIAN_POINT('',(0.7,-0.2,0.125));
#12567=CARTESIAN_POINT('',(0.7,-0.16,0.));
#12568=CARTESIAN_POINT('',(0.7,-0.1925,0.0325));
#12569=CARTESIAN_POINT('',(0.7,0.16,0.));
#12570=CARTESIAN_POINT('',(0.7,0.,0.));
#12571=CARTESIAN_POINT('',(0.7,0.2,0.04));
#12572=CARTESIAN_POINT('',(0.7,0.1925,0.0325));
#12573=CARTESIAN_POINT('',(0.7,0.2,0.125));
#12574=CARTESIAN_POINT('Origin',(-0.4,-0.18,0.02));
#12575=CARTESIAN_POINT('',(-0.7,-0.2,0.04));
#12576=CARTESIAN_POINT('',(-0.4,-0.2,0.04));
#12577=CARTESIAN_POINT('',(-0.7,-0.16,0.));
#12578=CARTESIAN_POINT('',(-0.7,-0.1925,0.0325));
#12579=CARTESIAN_POINT('',(-0.4,-0.16,0.));
#12580=CARTESIAN_POINT('Origin',(-0.8,-0.2,0.));
#12581=CARTESIAN_POINT('',(-0.7,-0.2,0.36));
#12582=CARTESIAN_POINT('',(-0.4,-0.2,0.36));
#12583=CARTESIAN_POINT('',(-0.7,-0.2,0.125));
#12584=CARTESIAN_POINT('Origin',(-0.4,-0.18,0.38));
#12585=CARTESIAN_POINT('',(-0.7,-0.16,0.4));
#12586=CARTESIAN_POINT('',(-0.4,-0.16,0.4));
#12587=CARTESIAN_POINT('',(-0.7,-0.1675,0.3925));
#12588=CARTESIAN_POINT('Origin',(0.,0.,0.4));
#12589=CARTESIAN_POINT('',(-0.7,0.16,0.4));
#12590=CARTESIAN_POINT('',(0.4,0.16,0.4));
#12591=CARTESIAN_POINT('',(-0.7,0.,0.4));
#12592=CARTESIAN_POINT('Origin',(-0.7,0.,0.25));
#12593=CARTESIAN_POINT('',(-0.7,0.2,0.36));
#12594=CARTESIAN_POINT('',(-0.7,0.1675,0.3925));
#12595=CARTESIAN_POINT('',(-0.7,0.2,0.04));
#12596=CARTESIAN_POINT('',(-0.7,0.2,0.125));
#12597=CARTESIAN_POINT('',(-0.7,0.16,0.));
#12598=CARTESIAN_POINT('',(-0.7,0.1925,0.0325));
#12599=CARTESIAN_POINT('',(-0.7,0.,0.));
#12600=CARTESIAN_POINT('Origin',(0.4,0.18,0.38));
#12601=CARTESIAN_POINT('',(0.4,0.2,0.36));
#12602=CARTESIAN_POINT('Origin',(0.8,0.2,0.));
#12603=CARTESIAN_POINT('',(0.4,0.2,0.04));
#12604=CARTESIAN_POINT('Origin',(0.4,0.18,0.02));
#12605=CARTESIAN_POINT('',(0.4,0.16,0.));
#12606=CARTESIAN_POINT('Origin',(0.,0.,0.));
#12607=CARTESIAN_POINT('',(0.,0.,0.));
#12608=CARTESIAN_POINT('Origin',(0.3,0.4,0.));
#12609=CARTESIAN_POINT('',(-0.3,0.4,-3.67394039744206E-17));
#12610=CARTESIAN_POINT('Origin',(0.,0.4,0.));
#12611=CARTESIAN_POINT('Origin',(0.,0.375,0.));
#12612=CARTESIAN_POINT('',(-0.35,0.35,-4.28626379701573E-17));
#12613=CARTESIAN_POINT('Origin',(0.,0.35,0.));
#12614=CARTESIAN_POINT('',(-0.325,0.375,-3.9801020972289E-17));
#12615=CARTESIAN_POINT('Origin',(0.,0.19,0.));
#12616=CARTESIAN_POINT('',(-0.35,0.03,-4.28626379701574E-17));
#12617=CARTESIAN_POINT('Origin',(0.,0.03,0.));
#12618=CARTESIAN_POINT('',(-0.35,0.19,-4.28626379701574E-17));
#12619=CARTESIAN_POINT('Origin',(0.,0.0149999999999999,0.));
#12620=CARTESIAN_POINT('',(-0.32,-3.29597460435593E-17,-3.91886975727153E-17));
#12621=CARTESIAN_POINT('Origin',(0.,0.,0.));
#12622=CARTESIAN_POINT('',(-0.335,0.0149999999999999,-4.10256677714363E-17));
#12623=CARTESIAN_POINT('Origin',(0.22,0.,0.));
#12624=CARTESIAN_POINT('',(-0.22,-6.93889390390723E-18,-2.69422295812418E-17));
#12625=CARTESIAN_POINT('Origin',(0.,0.,0.));
#12626=CARTESIAN_POINT('Origin',(0.,-0.02,0.));
#12627=CARTESIAN_POINT('',(-0.1954,-0.0492,2.39295984553393E-17));
#12628=CARTESIAN_POINT('Origin',(0.,-0.0492,0.));
#12629=CARTESIAN_POINT('',(-0.21,-0.02,-2.57175827820944E-17));
#12630=CARTESIAN_POINT('Origin',(0.,-0.8,0.));
#12631=CARTESIAN_POINT('',(-0.1954,-1.5646,2.39295984553393E-17));
#12632=CARTESIAN_POINT('Origin',(0.,-1.5646,0.));
#12633=CARTESIAN_POINT('',(-0.1954,-0.8,-2.39295984553393E-17));
#12634=CARTESIAN_POINT('Origin',(0.,-1.58,0.));
#12635=CARTESIAN_POINT('',(-0.16,-1.6,-1.95943487863577E-17));
#12636=CARTESIAN_POINT('Origin',(0.,-1.6,0.));
#12637=CARTESIAN_POINT('',(-0.18,-1.58,-2.20436423846524E-17));
#12638=CARTESIAN_POINT('Origin',(0.,-1.6,0.));
#12639=CARTESIAN_POINT('Origin',(0.0866025403784439,-0.4,-0.15));
#12640=CARTESIAN_POINT('',(0.173205080756888,-0.4,0.));
#12641=CARTESIAN_POINT('',(0.0866025403784439,-0.4,-0.15));
#12642=CARTESIAN_POINT('',(0.173205080756888,-0.4,0.));
#12643=CARTESIAN_POINT('',(0.0866025403784439,-0.64,-0.15));
#12644=CARTESIAN_POINT('',(0.0866025403784439,-0.4,-0.15));
#12645=CARTESIAN_POINT('',(0.173205080756888,-0.64,0.));
#12646=CARTESIAN_POINT('',(0.173205080756888,-0.64,0.));
#12647=CARTESIAN_POINT('',(0.173205080756888,-0.4,0.));
#12648=CARTESIAN_POINT('Origin',(-0.0866025403784438,-0.4,-0.15));
#12649=CARTESIAN_POINT('',(-0.0866025403784438,-0.4,-0.15));
#12650=CARTESIAN_POINT('',(0.0866025403784439,-0.4,-0.15));
#12651=CARTESIAN_POINT('',(-0.0866025403784438,-0.64,-0.15));
#12652=CARTESIAN_POINT('',(-0.0866025403784438,-0.4,-0.15));
#12653=CARTESIAN_POINT('',(0.0866025403784439,-0.64,-0.15));
#12654=CARTESIAN_POINT('Origin',(-0.173205080756888,-0.4,-2.77555756156289E-17));
#12655=CARTESIAN_POINT('',(-0.173205080756888,-0.4,-2.12115047744981E-17));
#12656=CARTESIAN_POINT('',(-0.0866025403784438,-0.4,-0.15));
#12657=CARTESIAN_POINT('',(-0.173205080756888,-0.64,-2.77555756156289E-17));
#12658=CARTESIAN_POINT('',(-0.173205080756888,-0.4,-2.12115047744981E-17));
#12659=CARTESIAN_POINT('',(-0.0866025403784438,-0.64,-0.15));
#12660=CARTESIAN_POINT('Origin',(-0.0866025403784439,-0.4,0.15));
#12661=CARTESIAN_POINT('',(-0.0866025403784439,-0.4,0.15));
#12662=CARTESIAN_POINT('',(-0.173205080756888,-0.4,-2.12115047744981E-17));
#12663=CARTESIAN_POINT('',(-0.0866025403784439,-0.64,0.15));
#12664=CARTESIAN_POINT('',(-0.0866025403784439,-0.4,0.15));
#12665=CARTESIAN_POINT('',(-0.173205080756888,-0.64,-2.12115047744981E-17));
#12666=CARTESIAN_POINT('Origin',(0.0866025403784439,-0.4,0.15));
#12667=CARTESIAN_POINT('',(0.0866025403784439,-0.4,0.15));
#12668=CARTESIAN_POINT('',(-0.0866025403784439,-0.4,0.15));
#12669=CARTESIAN_POINT('',(0.0866025403784439,-0.64,0.15));
#12670=CARTESIAN_POINT('',(0.0866025403784439,-0.4,0.15));
#12671=CARTESIAN_POINT('',(-0.0866025403784439,-0.64,0.15));
#12672=CARTESIAN_POINT('Origin',(0.173205080756888,-0.4,0.));
#12673=CARTESIAN_POINT('',(0.0866025403784439,-0.4,0.15));
#12674=CARTESIAN_POINT('',(0.0866025403784439,-0.64,0.15));
#12675=CARTESIAN_POINT('Origin',(0.,-0.4,-2.77555756156289E-17));
#12676=CARTESIAN_POINT('Origin',(0.,-0.64,-2.77555756156289E-17));
#12677=CARTESIAN_POINT('',(0.,0.,0.));
#12678=CARTESIAN_POINT('',(0.,0.,0.));
#12679=CARTESIAN_POINT('',(0.,0.,0.));
#12680=CARTESIAN_POINT('',(0.,0.,0.));
#12681=CARTESIAN_POINT('',(0.,0.,0.));
#12682=CARTESIAN_POINT('',(0.,0.,0.));
#12683=CARTESIAN_POINT('',(0.,0.,0.));
#12684=CARTESIAN_POINT('',(0.,0.,0.));
#12685=CARTESIAN_POINT('',(0.,0.,0.));
#12686=CARTESIAN_POINT('',(0.,0.,0.));
#12687=CARTESIAN_POINT('',(0.,0.,0.));
#12688=CARTESIAN_POINT('',(0.,0.,0.));
#12689=CARTESIAN_POINT('',(-3.,-2.5,1.8));
#12690=CARTESIAN_POINT('',(3.,-2.5,1.8));
#12691=CARTESIAN_POINT('',(0.,-2.5,4.));
#12692=CARTESIAN_POINT('',(1.4142135623731,-3.5,5.41421356237309));
#12693=CARTESIAN_POINT('',(-1.41421356237309,-3.5,5.41421356237309));
#12694=CARTESIAN_POINT('',(-1.4142135623731,-3.5,2.58578643762691));
#12695=CARTESIAN_POINT('',(1.41421356237309,-3.5,2.5857864376269));
#12696=CARTESIAN_POINT('',(1.4142135623731,-1.5,5.41421356237309));
#12697=CARTESIAN_POINT('',(-1.41421356237309,-1.5,5.41421356237309));
#12698=CARTESIAN_POINT('',(-1.4142135623731,-1.5,2.58578643762691));
#12699=CARTESIAN_POINT('',(1.41421356237309,-1.5,2.5857864376269));
#12700=CARTESIAN_POINT('',(-3.,2.5,1.8));
#12701=CARTESIAN_POINT('',(3.,2.5,1.8));
#12702=CARTESIAN_POINT('',(0.,2.5,4.));
#12703=CARTESIAN_POINT('',(1.4142135623731,1.5,5.41421356237309));
#12704=CARTESIAN_POINT('',(-1.4142135623731,1.5,5.41421356237309));
#12705=CARTESIAN_POINT('',(-1.4142135623731,1.5,2.58578643762691));
#12706=CARTESIAN_POINT('',(1.41421356237309,1.5,2.5857864376269));
#12707=CARTESIAN_POINT('',(1.4142135623731,3.5,5.41421356237309));
#12708=CARTESIAN_POINT('',(-1.41421356237309,3.5,5.41421356237309));
#12709=CARTESIAN_POINT('',(-1.4142135623731,3.5,2.58578643762691));
#12710=CARTESIAN_POINT('',(1.41421356237309,3.5,2.5857864376269));
#12711=CARTESIAN_POINT('',(-3.75,0.,2.4));
#12712=CARTESIAN_POINT('',(3.75,0.,2.4));
#12713=CARTESIAN_POINT('',(0.,0.,12.));
#12714=CARTESIAN_POINT('',(1.06066017177982,1.06066017177982,14.4));
#12715=CARTESIAN_POINT('',(-1.06066017177982,1.06066017177982,14.4));
#12716=CARTESIAN_POINT('',(-1.06066017177982,-1.06066017177982,14.4));
#12717=CARTESIAN_POINT('',(1.06066017177982,-1.06066017177982,14.4));
#12718=CARTESIAN_POINT('',(0.,0.,0.));
#12719=CARTESIAN_POINT('',(0.,0.,0.));
#12720=CARTESIAN_POINT('',(0.,0.,0.));
#12721=CARTESIAN_POINT('',(0.,0.,0.));
#12722=CARTESIAN_POINT('',(0.,0.,0.));
#12723=CARTESIAN_POINT('',(0.,0.,0.));
#12724=CARTESIAN_POINT('',(0.,0.,0.));
#12725=CARTESIAN_POINT('',(0.,0.,0.));
#12726=CARTESIAN_POINT('',(0.,0.,0.));
#12727=CARTESIAN_POINT('',(0.,0.,0.));
#12728=CARTESIAN_POINT('',(0.,0.,3.65));
#12729=CARTESIAN_POINT('',(-4.71342800766205E-31,5.5,3.65));
#12730=CARTESIAN_POINT('',(2.5,5.,4.));
#12731=CARTESIAN_POINT('',(0.,-4.7,4.));
#12732=CARTESIAN_POINT('',(0.,6.7,4.));
#12733=CARTESIAN_POINT('',(0.,0.,0.));
#12734=CARTESIAN_POINT('',(0.,0.,0.));
#12735=CARTESIAN_POINT('Origin',(0.,0.,6.3));
#12736=CARTESIAN_POINT('',(-0.425,-5.20474889637625E-17,6.4));
#12737=CARTESIAN_POINT('Origin',(0.,0.,6.4));
#12738=CARTESIAN_POINT('',(-0.425,5.20474889637625E-17,7.));
#12739=CARTESIAN_POINT('',(-0.425,-5.20474889637625E-17,6.3));
#12740=CARTESIAN_POINT('Origin',(0.,0.,7.));
#12741=CARTESIAN_POINT('Origin',(1.2,0.8,6.4));
#12742=CARTESIAN_POINT('',(1.2,0.8,6.4));
#12743=CARTESIAN_POINT('',(-1.2,0.8,6.4));
#12744=CARTESIAN_POINT('',(1.2,0.8,6.4));
#12745=CARTESIAN_POINT('',(-1.2,0.8,7.));
#12746=CARTESIAN_POINT('',(-1.2,0.8,6.4));
#12747=CARTESIAN_POINT('',(1.2,0.8,7.));
#12748=CARTESIAN_POINT('',(1.2,0.8,7.));
#12749=CARTESIAN_POINT('',(1.2,0.8,6.4));
#12750=CARTESIAN_POINT('Origin',(1.2,-0.8,6.4));
#12751=CARTESIAN_POINT('',(1.2,-0.8,6.4));
#12752=CARTESIAN_POINT('',(1.2,-0.8,6.4));
#12753=CARTESIAN_POINT('',(1.2,-0.8,7.));
#12754=CARTESIAN_POINT('',(1.2,-0.8,7.));
#12755=CARTESIAN_POINT('',(1.2,-0.8,6.4));
#12756=CARTESIAN_POINT('Origin',(-1.2,-0.8,6.4));
#12757=CARTESIAN_POINT('',(-1.2,-0.8,6.4));
#12758=CARTESIAN_POINT('',(-1.2,-0.8,6.4));
#12759=CARTESIAN_POINT('',(-1.2,-0.8,7.));
#12760=CARTESIAN_POINT('',(-1.2,-0.8,7.));
#12761=CARTESIAN_POINT('',(-1.2,-0.8,6.4));
#12762=CARTESIAN_POINT('Origin',(-1.2,0.8,6.4));
#12763=CARTESIAN_POINT('',(-1.2,0.8,6.4));
#12764=CARTESIAN_POINT('',(-1.2,0.8,7.));
#12765=CARTESIAN_POINT('Origin',(0.,0.,7.));
#12766=CARTESIAN_POINT('Origin',(0.,0.,6.4));
#12767=CARTESIAN_POINT('',(0.,0.,0.));
#12768=CARTESIAN_POINT('Origin',(0.,0.,16.));
#12769=CARTESIAN_POINT('',(-0.9,-1.10218211923262E-16,16.));
#12770=CARTESIAN_POINT('Origin',(0.,0.,16.));
#12771=CARTESIAN_POINT('',(-0.6,-7.34788079488412E-17,16.));
#12772=CARTESIAN_POINT('Origin',(0.,0.,16.));
#12773=CARTESIAN_POINT('Origin',(0.,0.,16.));
#12774=CARTESIAN_POINT('',(-0.9,-1.10218211923262E-16,16.5));
#12775=CARTESIAN_POINT('Origin',(0.,0.,16.5));
#12776=CARTESIAN_POINT('',(-0.9,-1.10218211923262E-16,16.));
#12777=CARTESIAN_POINT('Origin',(0.,0.,16.5));
#12778=CARTESIAN_POINT('Origin',(0.,0.,6.4));
#12779=CARTESIAN_POINT('',(-0.5,-6.12323399573677E-17,7.));
#12780=CARTESIAN_POINT('Origin',(0.,0.,7.));
#12781=CARTESIAN_POINT('',(-0.5,-6.12323399573677E-17,6.4));
#12782=CARTESIAN_POINT('',(-0.5,-6.12323399573677E-17,6.4));
#12783=CARTESIAN_POINT('Origin',(0.,0.,6.4));
#12784=CARTESIAN_POINT('Origin',(0.,0.,6.4));
#12785=CARTESIAN_POINT('Origin',(0.,0.,7.));
#12786=CARTESIAN_POINT('',(-0.6,-7.34788079488412E-17,7.));
#12787=CARTESIAN_POINT('',(-0.6,-7.34788079488412E-17,7.));
#12788=CARTESIAN_POINT('Origin',(0.,0.,7.));
#12789=CARTESIAN_POINT('Origin',(0.,0.,7.));
#12790=CARTESIAN_POINT('',(0.,0.,0.));
#12791=CARTESIAN_POINT('Origin',(0.,0.,7.));
#12792=CARTESIAN_POINT('',(-0.605,-7.40911313484149E-17,7.2));
#12793=CARTESIAN_POINT('Origin',(0.,0.,7.2));
#12794=CARTESIAN_POINT('',(-0.605,-7.40911313484149E-17,7.));
#12795=CARTESIAN_POINT('',(-0.605,-7.40911313484149E-17,7.));
#12796=CARTESIAN_POINT('Origin',(0.,0.,7.));
#12797=CARTESIAN_POINT('Origin',(0.,0.,7.));
#12798=CARTESIAN_POINT('',(-1.25,-1.53080849893419E-16,7.2));
#12799=CARTESIAN_POINT('Origin',(0.,0.,7.2));
#12800=CARTESIAN_POINT('',(-1.25,-1.53080849893419E-16,7.));
#12801=CARTESIAN_POINT('',(-1.25,-1.53080849893419E-16,7.));
#12802=CARTESIAN_POINT('Origin',(0.,0.,7.));
#12803=CARTESIAN_POINT('Origin',(0.,0.,7.2));
#12804=CARTESIAN_POINT('Origin',(0.,0.,7.));
#12805=CARTESIAN_POINT('',(0.,0.,0.));
#12806=CARTESIAN_POINT('',(0.,0.,0.));
#12807=CARTESIAN_POINT('',(0.,0.,0.));
#12808=CARTESIAN_POINT('',(0.,0.,0.));
#12809=CARTESIAN_POINT('',(0.,0.,0.));
#12810=CARTESIAN_POINT('',(0.,0.,0.));
#12811=UNCERTAINTY_MEASURE_WITH_UNIT(LENGTH_MEASURE(0.001),#12897,
'DISTANCE_ACCURACY_VALUE',
'Maximum model space distance between geometric entities at asserted c
onnectivities');
#12812=UNCERTAINTY_MEASURE_WITH_UNIT(LENGTH_MEASURE(0.001),#12897,
'DISTANCE_ACCURACY_VALUE',
'Maximum model space distance between geometric entities at asserted c
onnectivities');
#12813=UNCERTAINTY_MEASURE_WITH_UNIT(LENGTH_MEASURE(0.001),#12897,
'DISTANCE_ACCURACY_VALUE',
'Maximum model space distance between geometric entities at asserted c
onnectivities');
#12814=UNCERTAINTY_MEASURE_WITH_UNIT(LENGTH_MEASURE(0.001),#12897,
'DISTANCE_ACCURACY_VALUE',
'Maximum model space distance between geometric entities at asserted c
onnectivities');
#12815=UNCERTAINTY_MEASURE_WITH_UNIT(LENGTH_MEASURE(0.001),#12897,
'DISTANCE_ACCURACY_VALUE',
'Maximum model space distance between geometric entities at asserted c
onnectivities');
#12816=UNCERTAINTY_MEASURE_WITH_UNIT(LENGTH_MEASURE(0.001),#12897,
'DISTANCE_ACCURACY_VALUE',
'Maximum model space distance between geometric entities at asserted c
onnectivities');
#12817=UNCERTAINTY_MEASURE_WITH_UNIT(LENGTH_MEASURE(0.001),#12897,
'DISTANCE_ACCURACY_VALUE',
'Maximum model space distance between geometric entities at asserted c
onnectivities');
#12818=UNCERTAINTY_MEASURE_WITH_UNIT(LENGTH_MEASURE(0.001),#12897,
'DISTANCE_ACCURACY_VALUE',
'Maximum model space distance between geometric entities at asserted c
onnectivities');
#12819=UNCERTAINTY_MEASURE_WITH_UNIT(LENGTH_MEASURE(0.001),#12897,
'DISTANCE_ACCURACY_VALUE',
'Maximum model space distance between geometric entities at asserted c
onnectivities');
#12820=UNCERTAINTY_MEASURE_WITH_UNIT(LENGTH_MEASURE(0.001),#12897,
'DISTANCE_ACCURACY_VALUE',
'Maximum model space distance between geometric entities at asserted c
onnectivities');
#12821=UNCERTAINTY_MEASURE_WITH_UNIT(LENGTH_MEASURE(0.001),#12897,
'DISTANCE_ACCURACY_VALUE',
'Maximum model space distance between geometric entities at asserted c
onnectivities');
#12822=UNCERTAINTY_MEASURE_WITH_UNIT(LENGTH_MEASURE(0.001),#12897,
'DISTANCE_ACCURACY_VALUE',
'Maximum model space distance between geometric entities at asserted c
onnectivities');
#12823=UNCERTAINTY_MEASURE_WITH_UNIT(LENGTH_MEASURE(0.001),#12897,
'DISTANCE_ACCURACY_VALUE',
'Maximum model space distance between geometric entities at asserted c
onnectivities');
#12824=UNCERTAINTY_MEASURE_WITH_UNIT(LENGTH_MEASURE(0.001),#12897,
'DISTANCE_ACCURACY_VALUE',
'Maximum model space distance between geometric entities at asserted c
onnectivities');
#12825=UNCERTAINTY_MEASURE_WITH_UNIT(LENGTH_MEASURE(0.001),#12897,
'DISTANCE_ACCURACY_VALUE',
'Maximum model space distance between geometric entities at asserted c
onnectivities');
#12826=UNCERTAINTY_MEASURE_WITH_UNIT(LENGTH_MEASURE(0.001),#12897,
'DISTANCE_ACCURACY_VALUE',
'Maximum model space distance between geometric entities at asserted c
onnectivities');
#12827=UNCERTAINTY_MEASURE_WITH_UNIT(LENGTH_MEASURE(0.001),#12897,
'DISTANCE_ACCURACY_VALUE',
'Maximum model space distance between geometric entities at asserted c
onnectivities');
#12828=UNCERTAINTY_MEASURE_WITH_UNIT(LENGTH_MEASURE(0.001),#12897,
'DISTANCE_ACCURACY_VALUE',
'Maximum model space distance between geometric entities at asserted c
onnectivities');
#12829=UNCERTAINTY_MEASURE_WITH_UNIT(LENGTH_MEASURE(0.001),#12897,
'DISTANCE_ACCURACY_VALUE',
'Maximum model space distance between geometric entities at asserted c
onnectivities');
#12830=UNCERTAINTY_MEASURE_WITH_UNIT(LENGTH_MEASURE(0.001),#12897,
'DISTANCE_ACCURACY_VALUE',
'Maximum model space distance between geometric entities at asserted c
onnectivities');
#12831=UNCERTAINTY_MEASURE_WITH_UNIT(LENGTH_MEASURE(0.001),#12897,
'DISTANCE_ACCURACY_VALUE',
'Maximum model space distance between geometric entities at asserted c
onnectivities');
#12832=UNCERTAINTY_MEASURE_WITH_UNIT(LENGTH_MEASURE(0.001),#12897,
'DISTANCE_ACCURACY_VALUE',
'Maximum model space distance between geometric entities at asserted c
onnectivities');
#12833=UNCERTAINTY_MEASURE_WITH_UNIT(LENGTH_MEASURE(0.001),#12897,
'DISTANCE_ACCURACY_VALUE',
'Maximum model space distance between geometric entities at asserted c
onnectivities');
#12834=UNCERTAINTY_MEASURE_WITH_UNIT(LENGTH_MEASURE(0.001),#12897,
'DISTANCE_ACCURACY_VALUE',
'Maximum model space distance between geometric entities at asserted c
onnectivities');
#12835=UNCERTAINTY_MEASURE_WITH_UNIT(LENGTH_MEASURE(0.001),#12897,
'DISTANCE_ACCURACY_VALUE',
'Maximum model space distance between geometric entities at asserted c
onnectivities');
#12836=UNCERTAINTY_MEASURE_WITH_UNIT(LENGTH_MEASURE(0.001),#12897,
'DISTANCE_ACCURACY_VALUE',
'Maximum model space distance between geometric entities at asserted c
onnectivities');
#12837=UNCERTAINTY_MEASURE_WITH_UNIT(LENGTH_MEASURE(0.001),#12897,
'DISTANCE_ACCURACY_VALUE',
'Maximum model space distance between geometric entities at asserted c
onnectivities');
#12838=UNCERTAINTY_MEASURE_WITH_UNIT(LENGTH_MEASURE(0.001),#12897,
'DISTANCE_ACCURACY_VALUE',
'Maximum model space distance between geometric entities at asserted c
onnectivities');
#12839=UNCERTAINTY_MEASURE_WITH_UNIT(LENGTH_MEASURE(0.001),#12897,
'DISTANCE_ACCURACY_VALUE',
'Maximum model space distance between geometric entities at asserted c
onnectivities');
#12840=UNCERTAINTY_MEASURE_WITH_UNIT(LENGTH_MEASURE(0.001),#12897,
'DISTANCE_ACCURACY_VALUE',
'Maximum model space distance between geometric entities at asserted c
onnectivities');
#12841=UNCERTAINTY_MEASURE_WITH_UNIT(LENGTH_MEASURE(0.001),#12897,
'DISTANCE_ACCURACY_VALUE',
'Maximum model space distance between geometric entities at asserted c
onnectivities');
#12842=UNCERTAINTY_MEASURE_WITH_UNIT(LENGTH_MEASURE(0.001),#12897,
'DISTANCE_ACCURACY_VALUE',
'Maximum model space distance between geometric entities at asserted c
onnectivities');
#12843=UNCERTAINTY_MEASURE_WITH_UNIT(LENGTH_MEASURE(0.001),#12897,
'DISTANCE_ACCURACY_VALUE',
'Maximum model space distance between geometric entities at asserted c
onnectivities');
#12844=UNCERTAINTY_MEASURE_WITH_UNIT(LENGTH_MEASURE(0.001),#12897,
'DISTANCE_ACCURACY_VALUE',
'Maximum model space distance between geometric entities at asserted c
onnectivities');
#12845=UNCERTAINTY_MEASURE_WITH_UNIT(LENGTH_MEASURE(0.001),#12897,
'DISTANCE_ACCURACY_VALUE',
'Maximum model space distance between geometric entities at asserted c
onnectivities');
#12846=UNCERTAINTY_MEASURE_WITH_UNIT(LENGTH_MEASURE(0.001),#12897,
'DISTANCE_ACCURACY_VALUE',
'Maximum model space distance between geometric entities at asserted c
onnectivities');
#12847=UNCERTAINTY_MEASURE_WITH_UNIT(LENGTH_MEASURE(0.001),#12897,
'DISTANCE_ACCURACY_VALUE',
'Maximum model space distance between geometric entities at asserted c
onnectivities');
#12848=UNCERTAINTY_MEASURE_WITH_UNIT(LENGTH_MEASURE(0.001),#12897,
'DISTANCE_ACCURACY_VALUE',
'Maximum model space distance between geometric entities at asserted c
onnectivities');
#12849=UNCERTAINTY_MEASURE_WITH_UNIT(LENGTH_MEASURE(0.001),#12897,
'DISTANCE_ACCURACY_VALUE',
'Maximum model space distance between geometric entities at asserted c
onnectivities');
#12850=UNCERTAINTY_MEASURE_WITH_UNIT(LENGTH_MEASURE(0.001),#12897,
'DISTANCE_ACCURACY_VALUE',
'Maximum model space distance between geometric entities at asserted c
onnectivities');
#12851=UNCERTAINTY_MEASURE_WITH_UNIT(LENGTH_MEASURE(0.001),#12897,
'DISTANCE_ACCURACY_VALUE',
'Maximum model space distance between geometric entities at asserted c
onnectivities');
#12852=UNCERTAINTY_MEASURE_WITH_UNIT(LENGTH_MEASURE(0.001),#12897,
'DISTANCE_ACCURACY_VALUE',
'Maximum model space distance between geometric entities at asserted c
onnectivities');
#12853=UNCERTAINTY_MEASURE_WITH_UNIT(LENGTH_MEASURE(0.001),#12897,
'DISTANCE_ACCURACY_VALUE',
'Maximum model space distance between geometric entities at asserted c
onnectivities');
#12854=(
GEOMETRIC_REPRESENTATION_CONTEXT(3)
GLOBAL_UNCERTAINTY_ASSIGNED_CONTEXT((#12811))
GLOBAL_UNIT_ASSIGNED_CONTEXT((#12897,#12899,#12900))
REPRESENTATION_CONTEXT('','3D')
);
#12855=(
GEOMETRIC_REPRESENTATION_CONTEXT(3)
GLOBAL_UNCERTAINTY_ASSIGNED_CONTEXT((#12812))
GLOBAL_UNIT_ASSIGNED_CONTEXT((#12897,#12899,#12900))
REPRESENTATION_CONTEXT('','3D')
);
#12856=(
GEOMETRIC_REPRESENTATION_CONTEXT(3)
GLOBAL_UNCERTAINTY_ASSIGNED_CONTEXT((#12813))
GLOBAL_UNIT_ASSIGNED_CONTEXT((#12897,#12899,#12900))
REPRESENTATION_CONTEXT('','3D')
);
#12857=(
GEOMETRIC_REPRESENTATION_CONTEXT(3)
GLOBAL_UNCERTAINTY_ASSIGNED_CONTEXT((#12814))
GLOBAL_UNIT_ASSIGNED_CONTEXT((#12897,#12899,#12900))
REPRESENTATION_CONTEXT('','3D')
);
#12858=(
GEOMETRIC_REPRESENTATION_CONTEXT(3)
GLOBAL_UNCERTAINTY_ASSIGNED_CONTEXT((#12815))
GLOBAL_UNIT_ASSIGNED_CONTEXT((#12897,#12899,#12900))
REPRESENTATION_CONTEXT('','3D')
);
#12859=(
GEOMETRIC_REPRESENTATION_CONTEXT(3)
GLOBAL_UNCERTAINTY_ASSIGNED_CONTEXT((#12816))
GLOBAL_UNIT_ASSIGNED_CONTEXT((#12897,#12899,#12900))
REPRESENTATION_CONTEXT('','3D')
);
#12860=(
GEOMETRIC_REPRESENTATION_CONTEXT(3)
GLOBAL_UNCERTAINTY_ASSIGNED_CONTEXT((#12817))
GLOBAL_UNIT_ASSIGNED_CONTEXT((#12897,#12899,#12900))
REPRESENTATION_CONTEXT('','3D')
);
#12861=(
GEOMETRIC_REPRESENTATION_CONTEXT(3)
GLOBAL_UNCERTAINTY_ASSIGNED_CONTEXT((#12818))
GLOBAL_UNIT_ASSIGNED_CONTEXT((#12897,#12899,#12900))
REPRESENTATION_CONTEXT('','3D')
);
#12862=(
GEOMETRIC_REPRESENTATION_CONTEXT(3)
GLOBAL_UNCERTAINTY_ASSIGNED_CONTEXT((#12819))
GLOBAL_UNIT_ASSIGNED_CONTEXT((#12897,#12899,#12900))
REPRESENTATION_CONTEXT('','3D')
);
#12863=(
GEOMETRIC_REPRESENTATION_CONTEXT(3)
GLOBAL_UNCERTAINTY_ASSIGNED_CONTEXT((#12820))
GLOBAL_UNIT_ASSIGNED_CONTEXT((#12897,#12899,#12900))
REPRESENTATION_CONTEXT('','3D')
);
#12864=(
GEOMETRIC_REPRESENTATION_CONTEXT(3)
GLOBAL_UNCERTAINTY_ASSIGNED_CONTEXT((#12821))
GLOBAL_UNIT_ASSIGNED_CONTEXT((#12897,#12899,#12900))
REPRESENTATION_CONTEXT('','3D')
);
#12865=(
GEOMETRIC_REPRESENTATION_CONTEXT(3)
GLOBAL_UNCERTAINTY_ASSIGNED_CONTEXT((#12822))
GLOBAL_UNIT_ASSIGNED_CONTEXT((#12897,#12899,#12900))
REPRESENTATION_CONTEXT('','3D')
);
#12866=(
GEOMETRIC_REPRESENTATION_CONTEXT(3)
GLOBAL_UNCERTAINTY_ASSIGNED_CONTEXT((#12823))
GLOBAL_UNIT_ASSIGNED_CONTEXT((#12897,#12899,#12900))
REPRESENTATION_CONTEXT('','3D')
);
#12867=(
GEOMETRIC_REPRESENTATION_CONTEXT(3)
GLOBAL_UNCERTAINTY_ASSIGNED_CONTEXT((#12824))
GLOBAL_UNIT_ASSIGNED_CONTEXT((#12897,#12899,#12900))
REPRESENTATION_CONTEXT('','3D')
);
#12868=(
GEOMETRIC_REPRESENTATION_CONTEXT(3)
GLOBAL_UNCERTAINTY_ASSIGNED_CONTEXT((#12825))
GLOBAL_UNIT_ASSIGNED_CONTEXT((#12897,#12899,#12900))
REPRESENTATION_CONTEXT('','3D')
);
#12869=(
GEOMETRIC_REPRESENTATION_CONTEXT(3)
GLOBAL_UNCERTAINTY_ASSIGNED_CONTEXT((#12826))
GLOBAL_UNIT_ASSIGNED_CONTEXT((#12897,#12899,#12900))
REPRESENTATION_CONTEXT('','3D')
);
#12870=(
GEOMETRIC_REPRESENTATION_CONTEXT(3)
GLOBAL_UNCERTAINTY_ASSIGNED_CONTEXT((#12827))
GLOBAL_UNIT_ASSIGNED_CONTEXT((#12897,#12899,#12900))
REPRESENTATION_CONTEXT('','3D')
);
#12871=(
GEOMETRIC_REPRESENTATION_CONTEXT(3)
GLOBAL_UNCERTAINTY_ASSIGNED_CONTEXT((#12828))
GLOBAL_UNIT_ASSIGNED_CONTEXT((#12897,#12899,#12900))
REPRESENTATION_CONTEXT('','3D')
);
#12872=(
GEOMETRIC_REPRESENTATION_CONTEXT(3)
GLOBAL_UNCERTAINTY_ASSIGNED_CONTEXT((#12829))
GLOBAL_UNIT_ASSIGNED_CONTEXT((#12897,#12899,#12900))
REPRESENTATION_CONTEXT('','3D')
);
#12873=(
GEOMETRIC_REPRESENTATION_CONTEXT(3)
GLOBAL_UNCERTAINTY_ASSIGNED_CONTEXT((#12830))
GLOBAL_UNIT_ASSIGNED_CONTEXT((#12897,#12899,#12900))
REPRESENTATION_CONTEXT('','3D')
);
#12874=(
GEOMETRIC_REPRESENTATION_CONTEXT(3)
GLOBAL_UNCERTAINTY_ASSIGNED_CONTEXT((#12831))
GLOBAL_UNIT_ASSIGNED_CONTEXT((#12897,#12899,#12900))
REPRESENTATION_CONTEXT('','3D')
);
#12875=(
GEOMETRIC_REPRESENTATION_CONTEXT(3)
GLOBAL_UNCERTAINTY_ASSIGNED_CONTEXT((#12832))
GLOBAL_UNIT_ASSIGNED_CONTEXT((#12897,#12899,#12900))
REPRESENTATION_CONTEXT('','3D')
);
#12876=(
GEOMETRIC_REPRESENTATION_CONTEXT(3)
GLOBAL_UNCERTAINTY_ASSIGNED_CONTEXT((#12833))
GLOBAL_UNIT_ASSIGNED_CONTEXT((#12897,#12899,#12900))
REPRESENTATION_CONTEXT('','3D')
);
#12877=(
GEOMETRIC_REPRESENTATION_CONTEXT(3)
GLOBAL_UNCERTAINTY_ASSIGNED_CONTEXT((#12834))
GLOBAL_UNIT_ASSIGNED_CONTEXT((#12897,#12899,#12900))
REPRESENTATION_CONTEXT('','3D')
);
#12878=(
GEOMETRIC_REPRESENTATION_CONTEXT(3)
GLOBAL_UNCERTAINTY_ASSIGNED_CONTEXT((#12835))
GLOBAL_UNIT_ASSIGNED_CONTEXT((#12897,#12899,#12900))
REPRESENTATION_CONTEXT('','3D')
);
#12879=(
GEOMETRIC_REPRESENTATION_CONTEXT(3)
GLOBAL_UNCERTAINTY_ASSIGNED_CONTEXT((#12836))
GLOBAL_UNIT_ASSIGNED_CONTEXT((#12897,#12899,#12900))
REPRESENTATION_CONTEXT('','3D')
);
#12880=(
GEOMETRIC_REPRESENTATION_CONTEXT(3)
GLOBAL_UNCERTAINTY_ASSIGNED_CONTEXT((#12837))
GLOBAL_UNIT_ASSIGNED_CONTEXT((#12897,#12899,#12900))
REPRESENTATION_CONTEXT('','3D')
);
#12881=(
GEOMETRIC_REPRESENTATION_CONTEXT(3)
GLOBAL_UNCERTAINTY_ASSIGNED_CONTEXT((#12838))
GLOBAL_UNIT_ASSIGNED_CONTEXT((#12897,#12899,#12900))
REPRESENTATION_CONTEXT('','3D')
);
#12882=(
GEOMETRIC_REPRESENTATION_CONTEXT(3)
GLOBAL_UNCERTAINTY_ASSIGNED_CONTEXT((#12839))
GLOBAL_UNIT_ASSIGNED_CONTEXT((#12897,#12899,#12900))
REPRESENTATION_CONTEXT('','3D')
);
#12883=(
GEOMETRIC_REPRESENTATION_CONTEXT(3)
GLOBAL_UNCERTAINTY_ASSIGNED_CONTEXT((#12840))
GLOBAL_UNIT_ASSIGNED_CONTEXT((#12897,#12899,#12900))
REPRESENTATION_CONTEXT('','3D')
);
#12884=(
GEOMETRIC_REPRESENTATION_CONTEXT(3)
GLOBAL_UNCERTAINTY_ASSIGNED_CONTEXT((#12841))
GLOBAL_UNIT_ASSIGNED_CONTEXT((#12897,#12899,#12900))
REPRESENTATION_CONTEXT('','3D')
);
#12885=(
GEOMETRIC_REPRESENTATION_CONTEXT(3)
GLOBAL_UNCERTAINTY_ASSIGNED_CONTEXT((#12842))
GLOBAL_UNIT_ASSIGNED_CONTEXT((#12897,#12899,#12900))
REPRESENTATION_CONTEXT('','3D')
);
#12886=(
GEOMETRIC_REPRESENTATION_CONTEXT(3)
GLOBAL_UNCERTAINTY_ASSIGNED_CONTEXT((#12843))
GLOBAL_UNIT_ASSIGNED_CONTEXT((#12897,#12899,#12900))
REPRESENTATION_CONTEXT('','3D')
);
#12887=(
GEOMETRIC_REPRESENTATION_CONTEXT(3)
GLOBAL_UNCERTAINTY_ASSIGNED_CONTEXT((#12844))
GLOBAL_UNIT_ASSIGNED_CONTEXT((#12897,#12899,#12900))
REPRESENTATION_CONTEXT('','3D')
);
#12888=(
GEOMETRIC_REPRESENTATION_CONTEXT(3)
GLOBAL_UNCERTAINTY_ASSIGNED_CONTEXT((#12845))
GLOBAL_UNIT_ASSIGNED_CONTEXT((#12897,#12899,#12900))
REPRESENTATION_CONTEXT('','3D')
);
#12889=(
GEOMETRIC_REPRESENTATION_CONTEXT(3)
GLOBAL_UNCERTAINTY_ASSIGNED_CONTEXT((#12846))
GLOBAL_UNIT_ASSIGNED_CONTEXT((#12897,#12899,#12900))
REPRESENTATION_CONTEXT('','3D')
);
#12890=(
GEOMETRIC_REPRESENTATION_CONTEXT(3)
GLOBAL_UNCERTAINTY_ASSIGNED_CONTEXT((#12847))
GLOBAL_UNIT_ASSIGNED_CONTEXT((#12897,#12899,#12900))
REPRESENTATION_CONTEXT('','3D')
);
#12891=(
GEOMETRIC_REPRESENTATION_CONTEXT(3)
GLOBAL_UNCERTAINTY_ASSIGNED_CONTEXT((#12848))
GLOBAL_UNIT_ASSIGNED_CONTEXT((#12897,#12899,#12900))
REPRESENTATION_CONTEXT('','3D')
);
#12892=(
GEOMETRIC_REPRESENTATION_CONTEXT(3)
GLOBAL_UNCERTAINTY_ASSIGNED_CONTEXT((#12849))
GLOBAL_UNIT_ASSIGNED_CONTEXT((#12897,#12899,#12900))
REPRESENTATION_CONTEXT('','3D')
);
#12893=(
GEOMETRIC_REPRESENTATION_CONTEXT(3)
GLOBAL_UNCERTAINTY_ASSIGNED_CONTEXT((#12850))
GLOBAL_UNIT_ASSIGNED_CONTEXT((#12897,#12899,#12900))
REPRESENTATION_CONTEXT('','3D')
);
#12894=(
GEOMETRIC_REPRESENTATION_CONTEXT(3)
GLOBAL_UNCERTAINTY_ASSIGNED_CONTEXT((#12851))
GLOBAL_UNIT_ASSIGNED_CONTEXT((#12897,#12899,#12900))
REPRESENTATION_CONTEXT('','3D')
);
#12895=(
GEOMETRIC_REPRESENTATION_CONTEXT(3)
GLOBAL_UNCERTAINTY_ASSIGNED_CONTEXT((#12852))
GLOBAL_UNIT_ASSIGNED_CONTEXT((#12897,#12899,#12900))
REPRESENTATION_CONTEXT('','3D')
);
#12896=(
GEOMETRIC_REPRESENTATION_CONTEXT(3)
GLOBAL_UNCERTAINTY_ASSIGNED_CONTEXT((#12853))
GLOBAL_UNIT_ASSIGNED_CONTEXT((#12897,#12899,#12900))
REPRESENTATION_CONTEXT('','3D')
);
#12897=(
LENGTH_UNIT()
NAMED_UNIT(*)
SI_UNIT(.CENTI.,.METRE.)
);
#12898=(
LENGTH_UNIT()
NAMED_UNIT(*)
SI_UNIT($,.METRE.)
);
#12899=(
NAMED_UNIT(*)
PLANE_ANGLE_UNIT()
SI_UNIT($,.RADIAN.)
);
#12900=(
NAMED_UNIT(*)
SI_UNIT($,.STERADIAN.)
SOLID_ANGLE_UNIT()
);
#12901=SHAPE_DEFINITION_REPRESENTATION(#12943,#13054);
#12902=SHAPE_DEFINITION_REPRESENTATION(#12944,#13055);
#12903=SHAPE_DEFINITION_REPRESENTATION(#12945,#13056);
#12904=SHAPE_DEFINITION_REPRESENTATION(#12946,#13057);
#12905=SHAPE_DEFINITION_REPRESENTATION(#12947,#13058);
#12906=SHAPE_DEFINITION_REPRESENTATION(#12948,#13059);
#12907=SHAPE_DEFINITION_REPRESENTATION(#12949,#13060);
#12908=SHAPE_DEFINITION_REPRESENTATION(#12950,#13061);
#12909=SHAPE_DEFINITION_REPRESENTATION(#12951,#13062);
#12910=SHAPE_DEFINITION_REPRESENTATION(#12952,#13063);
#12911=SHAPE_DEFINITION_REPRESENTATION(#12953,#13064);
#12912=SHAPE_DEFINITION_REPRESENTATION(#12954,#13065);
#12913=SHAPE_DEFINITION_REPRESENTATION(#12955,#13066);
#12914=SHAPE_DEFINITION_REPRESENTATION(#12956,#13067);
#12915=SHAPE_DEFINITION_REPRESENTATION(#12957,#13068);
#12916=SHAPE_DEFINITION_REPRESENTATION(#12958,#13069);
#12917=SHAPE_DEFINITION_REPRESENTATION(#12959,#13070);
#12918=SHAPE_DEFINITION_REPRESENTATION(#12960,#13071);
#12919=SHAPE_DEFINITION_REPRESENTATION(#12961,#13072);
#12920=SHAPE_DEFINITION_REPRESENTATION(#12962,#13073);
#12921=SHAPE_DEFINITION_REPRESENTATION(#12968,#13074);
#12922=SHAPE_DEFINITION_REPRESENTATION(#12969,#13075);
#12923=SHAPE_DEFINITION_REPRESENTATION(#12970,#13076);
#12924=SHAPE_DEFINITION_REPRESENTATION(#12971,#13077);
#12925=SHAPE_DEFINITION_REPRESENTATION(#12974,#13078);
#12926=SHAPE_DEFINITION_REPRESENTATION(#12975,#13079);
#12927=SHAPE_DEFINITION_REPRESENTATION(#12976,#13080);
#12928=SHAPE_DEFINITION_REPRESENTATION(#12977,#13081);
#12929=SHAPE_DEFINITION_REPRESENTATION(#12978,#13082);
#12930=SHAPE_DEFINITION_REPRESENTATION(#12979,#13083);
#12931=SHAPE_DEFINITION_REPRESENTATION(#12980,#13084);
#12932=SHAPE_DEFINITION_REPRESENTATION(#12981,#13085);
#12933=SHAPE_DEFINITION_REPRESENTATION(#12982,#13086);
#12934=SHAPE_DEFINITION_REPRESENTATION(#12983,#13087);
#12935=SHAPE_DEFINITION_REPRESENTATION(#12984,#13088);
#12936=SHAPE_DEFINITION_REPRESENTATION(#12985,#13089);
#12937=SHAPE_DEFINITION_REPRESENTATION(#12986,#13090);
#12938=SHAPE_DEFINITION_REPRESENTATION(#12987,#13091);
#12939=SHAPE_DEFINITION_REPRESENTATION(#13044,#13092);
#12940=SHAPE_DEFINITION_REPRESENTATION(#13045,#13093);
#12941=SHAPE_DEFINITION_REPRESENTATION(#13046,#13094);
#12942=SHAPE_DEFINITION_REPRESENTATION(#13047,#13095);
#12943=PRODUCT_DEFINITION_SHAPE('',$,#13097);
#12944=PRODUCT_DEFINITION_SHAPE('',$,#13098);
#12945=PRODUCT_DEFINITION_SHAPE('',$,#13099);
#12946=PRODUCT_DEFINITION_SHAPE('',$,#13100);
#12947=PRODUCT_DEFINITION_SHAPE('',$,#13101);
#12948=PRODUCT_DEFINITION_SHAPE('',$,#13102);
#12949=PRODUCT_DEFINITION_SHAPE('',$,#13103);
#12950=PRODUCT_DEFINITION_SHAPE('',$,#13104);
#12951=PRODUCT_DEFINITION_SHAPE('',$,#13105);
#12952=PRODUCT_DEFINITION_SHAPE('',$,#13106);
#12953=PRODUCT_DEFINITION_SHAPE('',$,#13107);
#12954=PRODUCT_DEFINITION_SHAPE('',$,#13108);
#12955=PRODUCT_DEFINITION_SHAPE('',$,#13109);
#12956=PRODUCT_DEFINITION_SHAPE('',$,#13110);
#12957=PRODUCT_DEFINITION_SHAPE('',$,#13111);
#12958=PRODUCT_DEFINITION_SHAPE('',$,#13112);
#12959=PRODUCT_DEFINITION_SHAPE('',$,#13113);
#12960=PRODUCT_DEFINITION_SHAPE('',$,#13114);
#12961=PRODUCT_DEFINITION_SHAPE('',$,#13115);
#12962=PRODUCT_DEFINITION_SHAPE('',$,#13116);
#12963=PRODUCT_DEFINITION_SHAPE($,$,#224);
#12964=PRODUCT_DEFINITION_SHAPE($,$,#225);
#12965=PRODUCT_DEFINITION_SHAPE($,$,#226);
#12966=PRODUCT_DEFINITION_SHAPE($,$,#227);
#12967=PRODUCT_DEFINITION_SHAPE($,$,#228);
#12968=PRODUCT_DEFINITION_SHAPE('',$,#13117);
#12969=PRODUCT_DEFINITION_SHAPE('',$,#13118);
#12970=PRODUCT_DEFINITION_SHAPE('',$,#13119);
#12971=PRODUCT_DEFINITION_SHAPE('',$,#13120);
#12972=PRODUCT_DEFINITION_SHAPE($,$,#229);
#12973=PRODUCT_DEFINITION_SHAPE($,$,#230);
#12974=PRODUCT_DEFINITION_SHAPE('',$,#13121);
#12975=PRODUCT_DEFINITION_SHAPE('',$,#13122);
#12976=PRODUCT_DEFINITION_SHAPE('',$,#13123);
#12977=PRODUCT_DEFINITION_SHAPE('',$,#13124);
#12978=PRODUCT_DEFINITION_SHAPE('',$,#13125);
#12979=PRODUCT_DEFINITION_SHAPE('',$,#13126);
#12980=PRODUCT_DEFINITION_SHAPE('',$,#13127);
#12981=PRODUCT_DEFINITION_SHAPE('',$,#13128);
#12982=PRODUCT_DEFINITION_SHAPE('',$,#13129);
#12983=PRODUCT_DEFINITION_SHAPE('',$,#13130);
#12984=PRODUCT_DEFINITION_SHAPE('',$,#13131);
#12985=PRODUCT_DEFINITION_SHAPE('',$,#13132);
#12986=PRODUCT_DEFINITION_SHAPE('',$,#13133);
#12987=PRODUCT_DEFINITION_SHAPE('',$,#13134);
#12988=PRODUCT_DEFINITION_SHAPE($,$,#231);
#12989=PRODUCT_DEFINITION_SHAPE($,$,#232);
#12990=PRODUCT_DEFINITION_SHAPE($,$,#233);
#12991=PRODUCT_DEFINITION_SHAPE($,$,#234);
#12992=PRODUCT_DEFINITION_SHAPE($,$,#235);
#12993=PRODUCT_DEFINITION_SHAPE($,$,#236);
#12994=PRODUCT_DEFINITION_SHAPE($,$,#237);
#12995=PRODUCT_DEFINITION_SHAPE($,$,#238);
#12996=PRODUCT_DEFINITION_SHAPE($,$,#239);
#12997=PRODUCT_DEFINITION_SHAPE($,$,#240);
#12998=PRODUCT_DEFINITION_SHAPE($,$,#241);
#12999=PRODUCT_DEFINITION_SHAPE($,$,#242);
#13000=PRODUCT_DEFINITION_SHAPE($,$,#243);
#13001=PRODUCT_DEFINITION_SHAPE($,$,#244);
#13002=PRODUCT_DEFINITION_SHAPE($,$,#245);
#13003=PRODUCT_DEFINITION_SHAPE($,$,#246);
#13004=PRODUCT_DEFINITION_SHAPE($,$,#247);
#13005=PRODUCT_DEFINITION_SHAPE($,$,#248);
#13006=PRODUCT_DEFINITION_SHAPE($,$,#249);
#13007=PRODUCT_DEFINITION_SHAPE($,$,#250);
#13008=PRODUCT_DEFINITION_SHAPE($,$,#251);
#13009=PRODUCT_DEFINITION_SHAPE($,$,#252);
#13010=PRODUCT_DEFINITION_SHAPE($,$,#253);
#13011=PRODUCT_DEFINITION_SHAPE($,$,#254);
#13012=PRODUCT_DEFINITION_SHAPE($,$,#255);
#13013=PRODUCT_DEFINITION_SHAPE($,$,#256);
#13014=PRODUCT_DEFINITION_SHAPE($,$,#257);
#13015=PRODUCT_DEFINITION_SHAPE($,$,#258);
#13016=PRODUCT_DEFINITION_SHAPE($,$,#259);
#13017=PRODUCT_DEFINITION_SHAPE($,$,#260);
#13018=PRODUCT_DEFINITION_SHAPE($,$,#261);
#13019=PRODUCT_DEFINITION_SHAPE($,$,#262);
#13020=PRODUCT_DEFINITION_SHAPE($,$,#263);
#13021=PRODUCT_DEFINITION_SHAPE($,$,#264);
#13022=PRODUCT_DEFINITION_SHAPE($,$,#265);
#13023=PRODUCT_DEFINITION_SHAPE($,$,#266);
#13024=PRODUCT_DEFINITION_SHAPE($,$,#267);
#13025=PRODUCT_DEFINITION_SHAPE($,$,#268);
#13026=PRODUCT_DEFINITION_SHAPE($,$,#269);
#13027=PRODUCT_DEFINITION_SHAPE($,$,#270);
#13028=PRODUCT_DEFINITION_SHAPE($,$,#271);
#13029=PRODUCT_DEFINITION_SHAPE($,$,#272);
#13030=PRODUCT_DEFINITION_SHAPE($,$,#273);
#13031=PRODUCT_DEFINITION_SHAPE($,$,#274);
#13032=PRODUCT_DEFINITION_SHAPE($,$,#275);
#13033=PRODUCT_DEFINITION_SHAPE($,$,#276);
#13034=PRODUCT_DEFINITION_SHAPE($,$,#277);
#13035=PRODUCT_DEFINITION_SHAPE($,$,#278);
#13036=PRODUCT_DEFINITION_SHAPE($,$,#279);
#13037=PRODUCT_DEFINITION_SHAPE($,$,#280);
#13038=PRODUCT_DEFINITION_SHAPE($,$,#281);
#13039=PRODUCT_DEFINITION_SHAPE($,$,#282);
#13040=PRODUCT_DEFINITION_SHAPE($,$,#283);
#13041=PRODUCT_DEFINITION_SHAPE($,$,#284);
#13042=PRODUCT_DEFINITION_SHAPE($,$,#285);
#13043=PRODUCT_DEFINITION_SHAPE($,$,#286);
#13044=PRODUCT_DEFINITION_SHAPE('',$,#13135);
#13045=PRODUCT_DEFINITION_SHAPE('',$,#13136);
#13046=PRODUCT_DEFINITION_SHAPE('',$,#13137);
#13047=PRODUCT_DEFINITION_SHAPE('',$,#13138);
#13048=PRODUCT_DEFINITION_SHAPE($,$,#287);
#13049=PRODUCT_DEFINITION_SHAPE($,$,#288);
#13050=PRODUCT_DEFINITION_SHAPE($,$,#289);
#13051=PRODUCT_DEFINITION_SHAPE($,$,#290);
#13052=PRODUCT_DEFINITION_SHAPE($,$,#291);
#13053=PRODUCT_DEFINITION_SHAPE($,$,#292);
#13054=SHAPE_REPRESENTATION('',(#6622,#7411,#7412,#7413),#12854);
#13055=SHAPE_REPRESENTATION('',(#6623,#7318,#7319,#7320,#7321,#7322,#7323,
#7324,#7325,#7326,#7327,#7328,#7329,#7330,#7331,#7332,#7333,#7334,#7335,
#7336,#7337,#7338,#7339,#7340,#7341,#7342,#7343,#7344,#7345,#7346,#7347,
#7348,#7349,#7350,#7351,#7352,#7353,#7354,#7355,#7356,#7357,#7358),#12855);
#13056=SHAPE_REPRESENTATION('',(#6624),#12856);
#13057=SHAPE_REPRESENTATION('',(#6654),#12857);
#13058=SHAPE_REPRESENTATION('',(#6661),#12858);
#13059=SHAPE_REPRESENTATION('',(#6668),#12859);
#13060=SHAPE_REPRESENTATION('',(#6700),#12860);
#13061=SHAPE_REPRESENTATION('',(#6725),#12861);
#13062=SHAPE_REPRESENTATION('',(#6750),#12862);
#13063=SHAPE_REPRESENTATION('',(#6782),#12863);
#13064=SHAPE_REPRESENTATION('',(#6807),#12864);
#13065=SHAPE_REPRESENTATION('',(#6832),#12865);
#13066=SHAPE_REPRESENTATION('',(#6884),#12866);
#13067=SHAPE_REPRESENTATION('',(#6909),#12867);
#13068=SHAPE_REPRESENTATION('',(#6914,#7037,#7038,#7039,#7040,#7041),#12868);
#13069=SHAPE_REPRESENTATION('',(#6915),#12869);
#13070=SHAPE_REPRESENTATION('',(#6935),#12870);
#13071=SHAPE_REPRESENTATION('',(#6955),#12871);
#13072=SHAPE_REPRESENTATION('',(#6970),#12872);
#13073=SHAPE_REPRESENTATION('',(#7020),#12873);
#13074=SHAPE_REPRESENTATION('',(#7042),#12874);
#13075=SHAPE_REPRESENTATION('',(#7068,#7118,#7119),#12875);
#13076=SHAPE_REPRESENTATION('',(#7069),#12876);
#13077=SHAPE_REPRESENTATION('',(#7101),#12877);
#13078=SHAPE_REPRESENTATION('',(#7120),#12878);
#13079=SHAPE_REPRESENTATION('',(#7144,#7359,#7360,#7361,#7362,#7363,#7364,
#7365,#7366,#7367,#7368,#7369,#7370,#7371,#7372,#7373),#12879);
#13080=SHAPE_REPRESENTATION('',(#7145),#12880);
#13081=SHAPE_REPRESENTATION('',(#7173),#12881);
#13082=SHAPE_REPRESENTATION('',(#7182),#12882);
#13083=SHAPE_REPRESENTATION('',(#7191),#12883);
#13084=SHAPE_REPRESENTATION('',(#7200),#12884);
#13085=SHAPE_REPRESENTATION('',(#7209),#12885);
#13086=SHAPE_REPRESENTATION('',(#7229),#12886);
#13087=SHAPE_REPRESENTATION('',(#7253),#12887);
#13088=SHAPE_REPRESENTATION('',(#7263),#12888);
#13089=SHAPE_REPRESENTATION('',(#7272),#12889);
#13090=SHAPE_REPRESENTATION('',(#7281),#12890);
#13091=SHAPE_REPRESENTATION('',(#7292),#12891);
#13092=SHAPE_REPRESENTATION('',(#7374,#7408,#7409,#7410),#12892);
#13093=SHAPE_REPRESENTATION('',(#7375),#12893);
#13094=SHAPE_REPRESENTATION('',(#7385),#12894);
#13095=SHAPE_REPRESENTATION('',(#7399),#12895);
#13096=PRODUCT_DEFINITION_CONTEXT('part definition',#13224,'design');
#13097=PRODUCT_DEFINITION('PAT-017',
'PAT-017',#13139,#13096);
#13098=PRODUCT_DEFINITION('Bearing frame and stem guide',
'Bearing frame and stem guide',#13140,#13096);
#13099=PRODUCT_DEFINITION('Base','Base',#13141,#13096);
#13100=PRODUCT_DEFINITION('Foot','Foot',#13142,#13096);
#13101=PRODUCT_DEFINITION('Foot (1)','Foot (1)',#13143,#13096);
#13102=PRODUCT_DEFINITION('Camshaft bearing post',
'Camshaft bearing post',#13144,#13096);
#13103=PRODUCT_DEFINITION('Bearing cap','Bearing cap',#13145,#13096);
#13104=PRODUCT_DEFINITION('Bearing cap (1)','Bearing cap (1)',#13146,#13096);
#13105=PRODUCT_DEFINITION('Camshaft bearing post (1)',
'Camshaft bearing post (1)',#13147,#13096);
#13106=PRODUCT_DEFINITION('Bearing cap (2)','Bearing cap (2)',#13148,#13096);
#13107=PRODUCT_DEFINITION('Bearing cap (3)','Bearing cap (3)',#13149,#13096);
#13108=PRODUCT_DEFINITION('Valve guide bridge','Valve guide bridge',#13150,
#13096);
#13109=PRODUCT_DEFINITION('Stem guide cap','Stem guide cap',#13151,#13096);
#13110=PRODUCT_DEFINITION('Installed return spring',
'Installed return spring',#13152,#13096);
#13111=PRODUCT_DEFINITION('Sealed Ball Bearing - 12 x 32 x 10 mm',
'Sealed Ball Bearing - 12 x 32 x 10 mm',#13153,#13096);
#13112=PRODUCT_DEFINITION('Inner ring','Inner ring',#13154,#13096);
#13113=PRODUCT_DEFINITION('Outer ring','Outer ring',#13155,#13096);
#13114=PRODUCT_DEFINITION('Balls','Balls',#13156,#13096);
#13115=PRODUCT_DEFINITION('Cage','Cage',#13157,#13096);
#13116=PRODUCT_DEFINITION('Seals 2RS','Seals 2RS',#13158,#13096);
#13117=PRODUCT_DEFINITION('Cap Screw - M5x20','Cap Screw - M5x20',#13159,
#13096);
#13118=PRODUCT_DEFINITION('Linear Ball Bushing - 12 x 21 x 30 mm',
'Linear Ball Bushing - 12 x 21 x 30 mm',#13160,#13096);
#13119=PRODUCT_DEFINITION('Steel sleeve','Steel sleeve',#13161,#13096);
#13120=PRODUCT_DEFINITION('Ball retainer (plastic)',
'Ball retainer (plastic)',#13162,#13096);
#13121=PRODUCT_DEFINITION('M4x10 Cap Screw','M4x10 Cap Screw',#13163,#13096);
#13122=PRODUCT_DEFINITION('Camshaft and hand crank',
'Camshaft and hand crank',#13164,#13096);
#13123=PRODUCT_DEFINITION('Camshaft','Camshaft',#13165,#13096);
#13124=PRODUCT_DEFINITION('Inner race sleeve 10 mm',
'Inner race sleeve 10 mm',#13166,#13096);
#13125=PRODUCT_DEFINITION('Inner race sleeve 10 mm (1)',
'Inner race sleeve 10 mm (1)',#13167,#13096);
#13126=PRODUCT_DEFINITION('Inner race sleeve 15 mm',
'Inner race sleeve 15 mm',#13168,#13096);
#13127=PRODUCT_DEFINITION('Inner race sleeve 15 mm (1)',
'Inner race sleeve 15 mm (1)',#13169,#13096);
#13128=PRODUCT_DEFINITION('Eccentric cam','Eccentric cam',#13170,#13096);
#13129=PRODUCT_DEFINITION('Hand crank','Hand crank',#13171,#13096);
#13130=PRODUCT_DEFINITION('Crank grip','Crank grip',#13172,#13096);
#13131=PRODUCT_DEFINITION('Axial keeper','Axial keeper',#13173,#13096);
#13132=PRODUCT_DEFINITION('Axial keeper (1)','Axial keeper (1)',#13174,#13096);
#13133=PRODUCT_DEFINITION('Key 4x4x14','Key 4x4x14',#13175,#13096);
#13134=PRODUCT_DEFINITION('Cap Screw - M4x16','Cap Screw - M4x16',#13176,
#13096);
#13135=PRODUCT_DEFINITION('Valve stem and follower',
'Valve stem and follower',#13177,#13096);
#13136=PRODUCT_DEFINITION('Flat follower shoe','Flat follower shoe',#13178,
#13096);
#13137=PRODUCT_DEFINITION('Valve stem','Valve stem',#13179,#13096);
#13138=PRODUCT_DEFINITION('Spring seat washer','Spring seat washer',#13180,
#13096);
#13139=PRODUCT_DEFINITION_FORMATION('',$,#13226);
#13140=PRODUCT_DEFINITION_FORMATION('',$,#13227);
#13141=PRODUCT_DEFINITION_FORMATION('',$,#13228);
#13142=PRODUCT_DEFINITION_FORMATION('',$,#13229);
#13143=PRODUCT_DEFINITION_FORMATION('',$,#13230);
#13144=PRODUCT_DEFINITION_FORMATION('',$,#13231);
#13145=PRODUCT_DEFINITION_FORMATION('',$,#13232);
#13146=PRODUCT_DEFINITION_FORMATION('',$,#13233);
#13147=PRODUCT_DEFINITION_FORMATION('',$,#13234);
#13148=PRODUCT_DEFINITION_FORMATION('',$,#13235);
#13149=PRODUCT_DEFINITION_FORMATION('',$,#13236);
#13150=PRODUCT_DEFINITION_FORMATION('',$,#13237);
#13151=PRODUCT_DEFINITION_FORMATION('',$,#13238);
#13152=PRODUCT_DEFINITION_FORMATION('',$,#13239);
#13153=PRODUCT_DEFINITION_FORMATION('',$,#13240);
#13154=PRODUCT_DEFINITION_FORMATION('',$,#13241);
#13155=PRODUCT_DEFINITION_FORMATION('',$,#13242);
#13156=PRODUCT_DEFINITION_FORMATION('',$,#13243);
#13157=PRODUCT_DEFINITION_FORMATION('',$,#13244);
#13158=PRODUCT_DEFINITION_FORMATION('',$,#13245);
#13159=PRODUCT_DEFINITION_FORMATION('',$,#13246);
#13160=PRODUCT_DEFINITION_FORMATION('',$,#13247);
#13161=PRODUCT_DEFINITION_FORMATION('',$,#13248);
#13162=PRODUCT_DEFINITION_FORMATION('',$,#13249);
#13163=PRODUCT_DEFINITION_FORMATION('',$,#13250);
#13164=PRODUCT_DEFINITION_FORMATION('',$,#13251);
#13165=PRODUCT_DEFINITION_FORMATION('',$,#13252);
#13166=PRODUCT_DEFINITION_FORMATION('',$,#13253);
#13167=PRODUCT_DEFINITION_FORMATION('',$,#13254);
#13168=PRODUCT_DEFINITION_FORMATION('',$,#13255);
#13169=PRODUCT_DEFINITION_FORMATION('',$,#13256);
#13170=PRODUCT_DEFINITION_FORMATION('',$,#13257);
#13171=PRODUCT_DEFINITION_FORMATION('',$,#13258);
#13172=PRODUCT_DEFINITION_FORMATION('',$,#13259);
#13173=PRODUCT_DEFINITION_FORMATION('',$,#13260);
#13174=PRODUCT_DEFINITION_FORMATION('',$,#13261);
#13175=PRODUCT_DEFINITION_FORMATION('',$,#13262);
#13176=PRODUCT_DEFINITION_FORMATION('',$,#13263);
#13177=PRODUCT_DEFINITION_FORMATION('',$,#13264);
#13178=PRODUCT_DEFINITION_FORMATION('',$,#13265);
#13179=PRODUCT_DEFINITION_FORMATION('',$,#13266);
#13180=PRODUCT_DEFINITION_FORMATION('',$,#13267);
#13181=PRODUCT_RELATED_PRODUCT_CATEGORY('PAT-017','PAT-017',(#13226));
#13182=PRODUCT_RELATED_PRODUCT_CATEGORY('Bearing frame and stem guide',
'Bearing frame and stem guide',(#13227));
#13183=PRODUCT_RELATED_PRODUCT_CATEGORY('Base','Base',(#13228));
#13184=PRODUCT_RELATED_PRODUCT_CATEGORY('Foot','Foot',(#13229));
#13185=PRODUCT_RELATED_PRODUCT_CATEGORY('Foot (1)','Foot (1)',(#13230));
#13186=PRODUCT_RELATED_PRODUCT_CATEGORY('Camshaft bearing post',
'Camshaft bearing post',(#13231));
#13187=PRODUCT_RELATED_PRODUCT_CATEGORY('Bearing cap','Bearing cap',(#13232));
#13188=PRODUCT_RELATED_PRODUCT_CATEGORY('Bearing cap (1)',
'Bearing cap (1)',(#13233));
#13189=PRODUCT_RELATED_PRODUCT_CATEGORY('Camshaft bearing post (1)',
'Camshaft bearing post (1)',(#13234));
#13190=PRODUCT_RELATED_PRODUCT_CATEGORY('Bearing cap (2)',
'Bearing cap (2)',(#13235));
#13191=PRODUCT_RELATED_PRODUCT_CATEGORY('Bearing cap (3)',
'Bearing cap (3)',(#13236));
#13192=PRODUCT_RELATED_PRODUCT_CATEGORY('Valve guide bridge',
'Valve guide bridge',(#13237));
#13193=PRODUCT_RELATED_PRODUCT_CATEGORY('Stem guide cap',
'Stem guide cap',(#13238));
#13194=PRODUCT_RELATED_PRODUCT_CATEGORY('Installed return spring',
'Installed return spring',(#13239));
#13195=PRODUCT_RELATED_PRODUCT_CATEGORY(
'Sealed Ball Bearing - 12 x 32 x 10 mm',
'Sealed Ball Bearing - 12 x 32 x 10 mm',(#13240));
#13196=PRODUCT_RELATED_PRODUCT_CATEGORY('Inner ring','Inner ring',(#13241));
#13197=PRODUCT_RELATED_PRODUCT_CATEGORY('Outer ring','Outer ring',(#13242));
#13198=PRODUCT_RELATED_PRODUCT_CATEGORY('Balls','Balls',(#13243));
#13199=PRODUCT_RELATED_PRODUCT_CATEGORY('Cage','Cage',(#13244));
#13200=PRODUCT_RELATED_PRODUCT_CATEGORY('Seals 2RS','Seals 2RS',(#13245));
#13201=PRODUCT_RELATED_PRODUCT_CATEGORY('Cap Screw - M5x20',
'Cap Screw - M5x20',(#13246));
#13202=PRODUCT_RELATED_PRODUCT_CATEGORY(
'Linear Ball Bushing - 12 x 21 x 30 mm',
'Linear Ball Bushing - 12 x 21 x 30 mm',(#13247));
#13203=PRODUCT_RELATED_PRODUCT_CATEGORY('Steel sleeve','Steel sleeve',(#13248));
#13204=PRODUCT_RELATED_PRODUCT_CATEGORY('Ball retainer (plastic)',
'Ball retainer (plastic)',(#13249));
#13205=PRODUCT_RELATED_PRODUCT_CATEGORY('M4x10 Cap Screw',
'M4x10 Cap Screw',(#13250));
#13206=PRODUCT_RELATED_PRODUCT_CATEGORY('Camshaft and hand crank',
'Camshaft and hand crank',(#13251));
#13207=PRODUCT_RELATED_PRODUCT_CATEGORY('Camshaft','Camshaft',(#13252));
#13208=PRODUCT_RELATED_PRODUCT_CATEGORY('Inner race sleeve 10 mm',
'Inner race sleeve 10 mm',(#13253));
#13209=PRODUCT_RELATED_PRODUCT_CATEGORY('Inner race sleeve 10 mm (1)',
'Inner race sleeve 10 mm (1)',(#13254));
#13210=PRODUCT_RELATED_PRODUCT_CATEGORY('Inner race sleeve 15 mm',
'Inner race sleeve 15 mm',(#13255));
#13211=PRODUCT_RELATED_PRODUCT_CATEGORY('Inner race sleeve 15 mm (1)',
'Inner race sleeve 15 mm (1)',(#13256));
#13212=PRODUCT_RELATED_PRODUCT_CATEGORY('Eccentric cam','Eccentric cam',
(#13257));
#13213=PRODUCT_RELATED_PRODUCT_CATEGORY('Hand crank','Hand crank',(#13258));
#13214=PRODUCT_RELATED_PRODUCT_CATEGORY('Crank grip','Crank grip',(#13259));
#13215=PRODUCT_RELATED_PRODUCT_CATEGORY('Axial keeper','Axial keeper',(#13260));
#13216=PRODUCT_RELATED_PRODUCT_CATEGORY('Axial keeper (1)',
'Axial keeper (1)',(#13261));
#13217=PRODUCT_RELATED_PRODUCT_CATEGORY('Key 4x4x14','Key 4x4x14',(#13262));
#13218=PRODUCT_RELATED_PRODUCT_CATEGORY('Cap Screw - M4x16',
'Cap Screw - M4x16',(#13263));
#13219=PRODUCT_RELATED_PRODUCT_CATEGORY('Valve stem and follower',
'Valve stem and follower',(#13264));
#13220=PRODUCT_RELATED_PRODUCT_CATEGORY('Flat follower shoe',
'Flat follower shoe',(#13265));
#13221=PRODUCT_RELATED_PRODUCT_CATEGORY('Valve stem','Valve stem',(#13266));
#13222=PRODUCT_RELATED_PRODUCT_CATEGORY('Spring seat washer',
'Spring seat washer',(#13267));
#13223=APPLICATION_PROTOCOL_DEFINITION('international standard',
'automotive_design',2009,#13224);
#13224=APPLICATION_CONTEXT(
'Core Data for Automotive Mechanical Design Process');
#13225=PRODUCT_CONTEXT('part definition',#13224,'mechanical');
#13226=PRODUCT('PAT-017','PAT-017',
'PAT-017',(#13225));
#13227=PRODUCT('Bearing frame and stem guide',
'Bearing frame and stem guide','Bearing frame and stem guide',(#13225));
#13228=PRODUCT('Base','Base','Base',(#13225));
#13229=PRODUCT('Foot','Foot','Foot',(#13225));
#13230=PRODUCT('Foot (1)','Foot (1)','Foot (1)',(#13225));
#13231=PRODUCT('Camshaft bearing post','Camshaft bearing post',
'Camshaft bearing post',(#13225));
#13232=PRODUCT('Bearing cap','Bearing cap','Bearing cap',(#13225));
#13233=PRODUCT('Bearing cap (1)','Bearing cap (1)','Bearing cap (1)',(#13225));
#13234=PRODUCT('Camshaft bearing post (1)','Camshaft bearing post (1)',
'Camshaft bearing post (1)',(#13225));
#13235=PRODUCT('Bearing cap (2)','Bearing cap (2)','Bearing cap (2)',(#13225));
#13236=PRODUCT('Bearing cap (3)','Bearing cap (3)','Bearing cap (3)',(#13225));
#13237=PRODUCT('Valve guide bridge','Valve guide bridge',
'Valve guide bridge',(#13225));
#13238=PRODUCT('Stem guide cap','Stem guide cap','Stem guide cap',(#13225));
#13239=PRODUCT('Installed return spring','Installed return spring',
'Installed return spring',(#13225));
#13240=PRODUCT('Sealed Ball Bearing - 12 x 32 x 10 mm',
'Sealed Ball Bearing - 12 x 32 x 10 mm',
'Sealed Ball Bearing - 12 x 32 x 10 mm',(#13225));
#13241=PRODUCT('Inner ring','Inner ring','Inner ring',(#13225));
#13242=PRODUCT('Outer ring','Outer ring','Outer ring',(#13225));
#13243=PRODUCT('Balls','Balls','Balls',(#13225));
#13244=PRODUCT('Cage','Cage','Cage',(#13225));
#13245=PRODUCT('Seals 2RS','Seals 2RS','Seals 2RS',(#13225));
#13246=PRODUCT('Cap Screw - M5x20','Cap Screw - M5x20',
'Cap Screw - M5x20',(#13225));
#13247=PRODUCT('Linear Ball Bushing - 12 x 21 x 30 mm',
'Linear Ball Bushing - 12 x 21 x 30 mm',
'Linear Ball Bushing - 12 x 21 x 30 mm',(#13225));
#13248=PRODUCT('Steel sleeve','Steel sleeve','Steel sleeve',(#13225));
#13249=PRODUCT('Ball retainer (plastic)','Ball retainer (plastic)',
'Ball retainer (plastic)',(#13225));
#13250=PRODUCT('M4x10 Cap Screw','M4x10 Cap Screw','M4x10 Cap Screw',(#13225));
#13251=PRODUCT('Camshaft and hand crank','Camshaft and hand crank',
'Camshaft and hand crank',(#13225));
#13252=PRODUCT('Camshaft','Camshaft','Camshaft',(#13225));
#13253=PRODUCT('Inner race sleeve 10 mm','Inner race sleeve 10 mm',
'Inner race sleeve 10 mm',(#13225));
#13254=PRODUCT('Inner race sleeve 10 mm (1)',
'Inner race sleeve 10 mm (1)','Inner race sleeve 10 mm (1)',(#13225));
#13255=PRODUCT('Inner race sleeve 15 mm','Inner race sleeve 15 mm',
'Inner race sleeve 15 mm',(#13225));
#13256=PRODUCT('Inner race sleeve 15 mm (1)',
'Inner race sleeve 15 mm (1)','Inner race sleeve 15 mm (1)',(#13225));
#13257=PRODUCT('Eccentric cam','Eccentric cam','Eccentric cam',(#13225));
#13258=PRODUCT('Hand crank','Hand crank','Hand crank',(#13225));
#13259=PRODUCT('Crank grip','Crank grip','Crank grip',(#13225));
#13260=PRODUCT('Axial keeper','Axial keeper','Axial keeper',(#13225));
#13261=PRODUCT('Axial keeper (1)','Axial keeper (1)','Axial keeper (1)',(#13225));
#13262=PRODUCT('Key 4x4x14','Key 4x4x14','Key 4x4x14',(#13225));
#13263=PRODUCT('Cap Screw - M4x16','Cap Screw - M4x16',
'Cap Screw - M4x16',(#13225));
#13264=PRODUCT('Valve stem and follower','Valve stem and follower',
'Valve stem and follower',(#13225));
#13265=PRODUCT('Flat follower shoe','Flat follower shoe',
'Flat follower shoe',(#13225));
#13266=PRODUCT('Valve stem','Valve stem','Valve stem',(#13225));
#13267=PRODUCT('Spring seat washer','Spring seat washer',
'Spring seat washer',(#13225));
#13268=PRESENTATION_STYLE_ASSIGNMENT((#13273));
#13269=PRESENTATION_STYLE_ASSIGNMENT((#13274));
#13270=PRESENTATION_STYLE_ASSIGNMENT((#13275));
#13271=PRESENTATION_STYLE_ASSIGNMENT((#13276));
#13272=PRESENTATION_STYLE_ASSIGNMENT((#13277));
#13273=SURFACE_STYLE_USAGE(.BOTH.,#13278);
#13274=SURFACE_STYLE_USAGE(.BOTH.,#13279);
#13275=SURFACE_STYLE_USAGE(.BOTH.,#13280);
#13276=SURFACE_STYLE_USAGE(.BOTH.,#13281);
#13277=SURFACE_STYLE_USAGE(.BOTH.,#13282);
#13278=SURFACE_SIDE_STYLE('',(#13283));
#13279=SURFACE_SIDE_STYLE('',(#13284));
#13280=SURFACE_SIDE_STYLE('',(#13285));
#13281=SURFACE_SIDE_STYLE('',(#13286));
#13282=SURFACE_SIDE_STYLE('',(#13287));
#13283=SURFACE_STYLE_FILL_AREA(#13288);
#13284=SURFACE_STYLE_FILL_AREA(#13289);
#13285=SURFACE_STYLE_FILL_AREA(#13290);
#13286=SURFACE_STYLE_FILL_AREA(#13291);
#13287=SURFACE_STYLE_FILL_AREA(#13292);
#13288=FILL_AREA_STYLE('Steel - Satin',(#13293));
#13289=FILL_AREA_STYLE('CAD Library Painted - Deep blue',(#13294));
#13290=FILL_AREA_STYLE('CAD Library Painted - Steel gray',(#13295));
#13291=FILL_AREA_STYLE('CAD Library Painted - Engineering blue',(#13296));
#13292=FILL_AREA_STYLE('CAD Library Painted - Graphite',(#13297));
#13293=FILL_AREA_STYLE_COLOUR('Steel - Satin',#13298);
#13294=FILL_AREA_STYLE_COLOUR('CAD Library Painted - Deep blue',#13299);
#13295=FILL_AREA_STYLE_COLOUR('CAD Library Painted - Steel gray',#13300);
#13296=FILL_AREA_STYLE_COLOUR('CAD Library Painted - Engineering blue',
#13301);
#13297=FILL_AREA_STYLE_COLOUR('CAD Library Painted - Graphite',#13302);
#13298=COLOUR_RGB('Steel - Satin',0.627450980392157,0.627450980392157,0.627450980392157);
#13299=COLOUR_RGB('CAD Library Painted - Deep blue',0.0784313725490196,
0.203921568627451,0.349019607843137);
#13300=COLOUR_RGB('CAD Library Painted - Steel gray',0.592156862745098,
0.631372549019608,0.67843137254902);
#13301=COLOUR_RGB('CAD Library Painted - Engineering blue',0.12156862745098,
0.356862745098039,0.6);
#13302=COLOUR_RGB('CAD Library Painted - Graphite',0.168627450980392,0.192156862745098,
0.231372549019608);
#13303=COLOUR_RGB('Dark Blue',0.08,0.2,0.34);
#13304=FILL_AREA_STYLE_COLOUR('',#13303);
#13305=FILL_AREA_STYLE('',(#13304));
#13306=SURFACE_STYLE_FILL_AREA(#13305);
#13307=SURFACE_SIDE_STYLE('',(#13306));
#13308=SURFACE_STYLE_USAGE(.BOTH.,#13307);
#13309=PRESENTATION_STYLE_ASSIGNMENT((#13308));
#13310=COLOUR_RGB('Light Blue',0.38,0.62,0.78);
#13311=FILL_AREA_STYLE_COLOUR('',#13310);
#13312=FILL_AREA_STYLE('',(#13311));
#13313=SURFACE_STYLE_FILL_AREA(#13312);
#13314=SURFACE_SIDE_STYLE('',(#13313));
#13315=SURFACE_STYLE_USAGE(.BOTH.,#13314);
#13316=PRESENTATION_STYLE_ASSIGNMENT((#13315));
#13317=COLOUR_RGB('Sky Blue',0.24,0.69,0.87);
#13318=FILL_AREA_STYLE_COLOUR('',#13317);
#13319=FILL_AREA_STYLE('',(#13318));
#13320=SURFACE_STYLE_FILL_AREA(#13319);
#13321=SURFACE_SIDE_STYLE('',(#13320));
#13322=SURFACE_STYLE_USAGE(.BOTH.,#13321);
#13323=PRESENTATION_STYLE_ASSIGNMENT((#13322));
#13324=COLOUR_RGB('Grey',0.48,0.52,0.57);
#13325=FILL_AREA_STYLE_COLOUR('',#13324);
#13326=FILL_AREA_STYLE('',(#13325));
#13327=SURFACE_STYLE_FILL_AREA(#13326);
#13328=SURFACE_SIDE_STYLE('',(#13327));
#13329=SURFACE_STYLE_USAGE(.BOTH.,#13328);
#13330=PRESENTATION_STYLE_ASSIGNMENT((#13329));
#13331=COLOUR_RGB('Black',0.12,0.14,0.17);
#13332=FILL_AREA_STYLE_COLOUR('',#13331);
#13333=FILL_AREA_STYLE('',(#13332));
#13334=SURFACE_STYLE_FILL_AREA(#13333);
#13335=SURFACE_SIDE_STYLE('',(#13334));
#13336=SURFACE_STYLE_USAGE(.BOTH.,#13335);
#13337=PRESENTATION_STYLE_ASSIGNMENT((#13336));
#13338=COLOUR_RGB('Off White',0.89,0.88,0.83);
#13339=FILL_AREA_STYLE_COLOUR('',#13338);
#13340=FILL_AREA_STYLE('',(#13339));
#13341=SURFACE_STYLE_FILL_AREA(#13340);
#13342=SURFACE_SIDE_STYLE('',(#13341));
#13343=SURFACE_STYLE_USAGE(.BOTH.,#13342);
#13344=PRESENTATION_STYLE_ASSIGNMENT((#13343));
ENDSEC;
END-ISO-10303-21;
